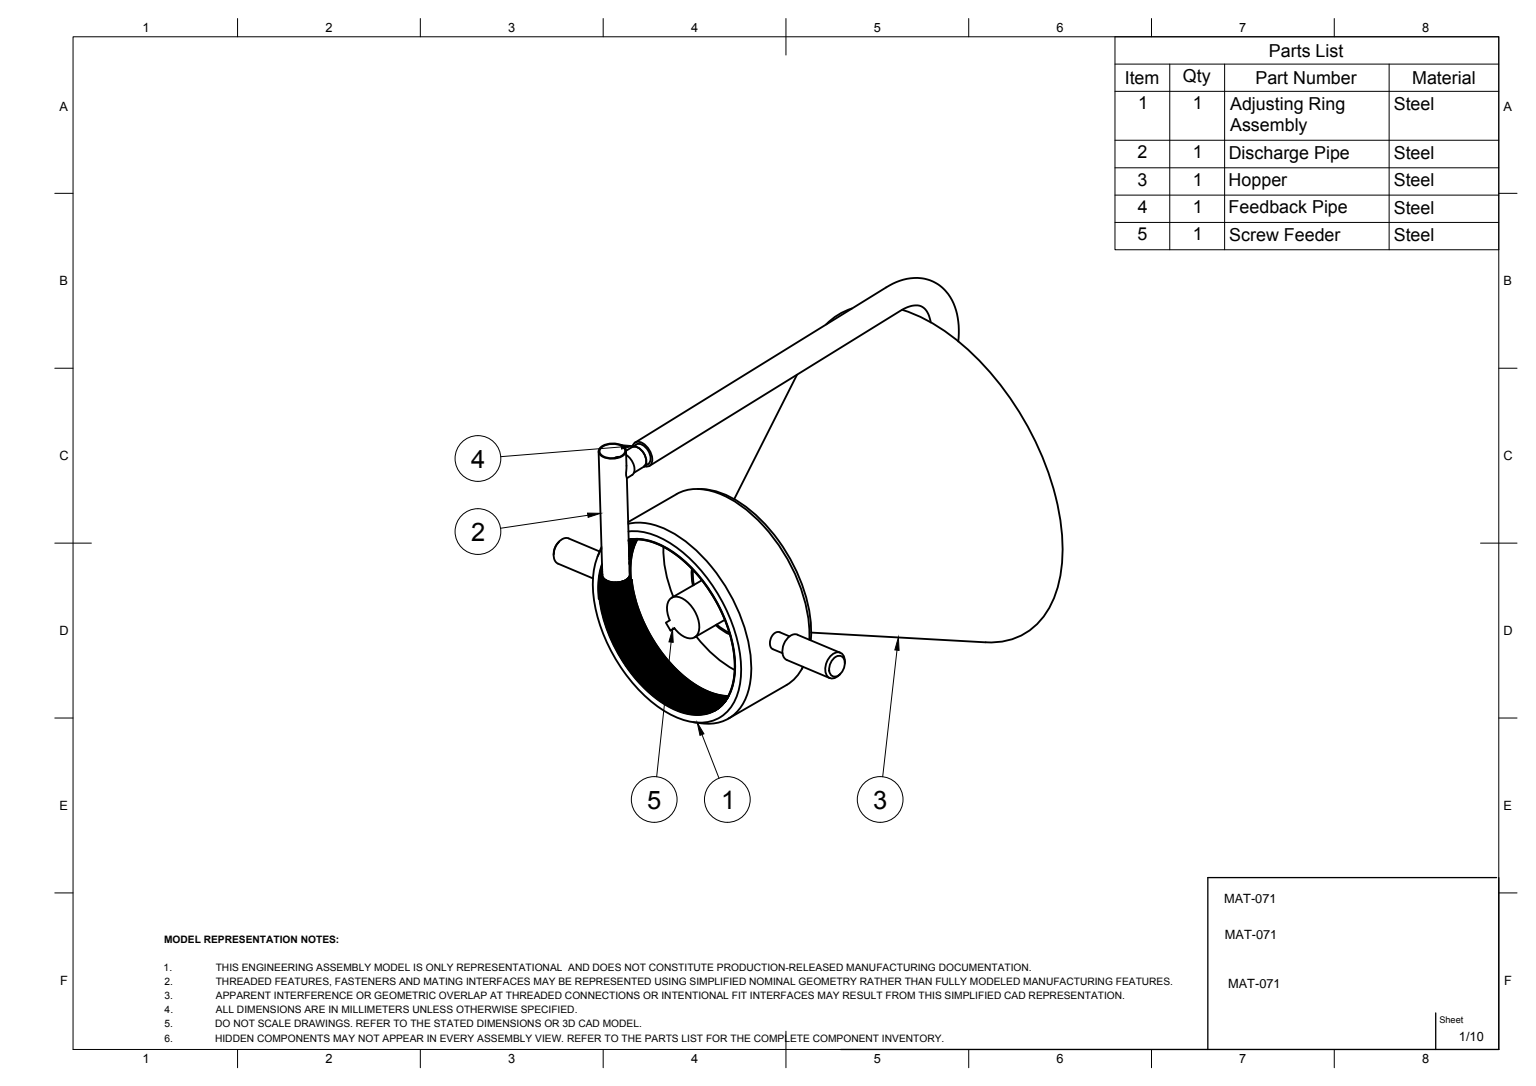
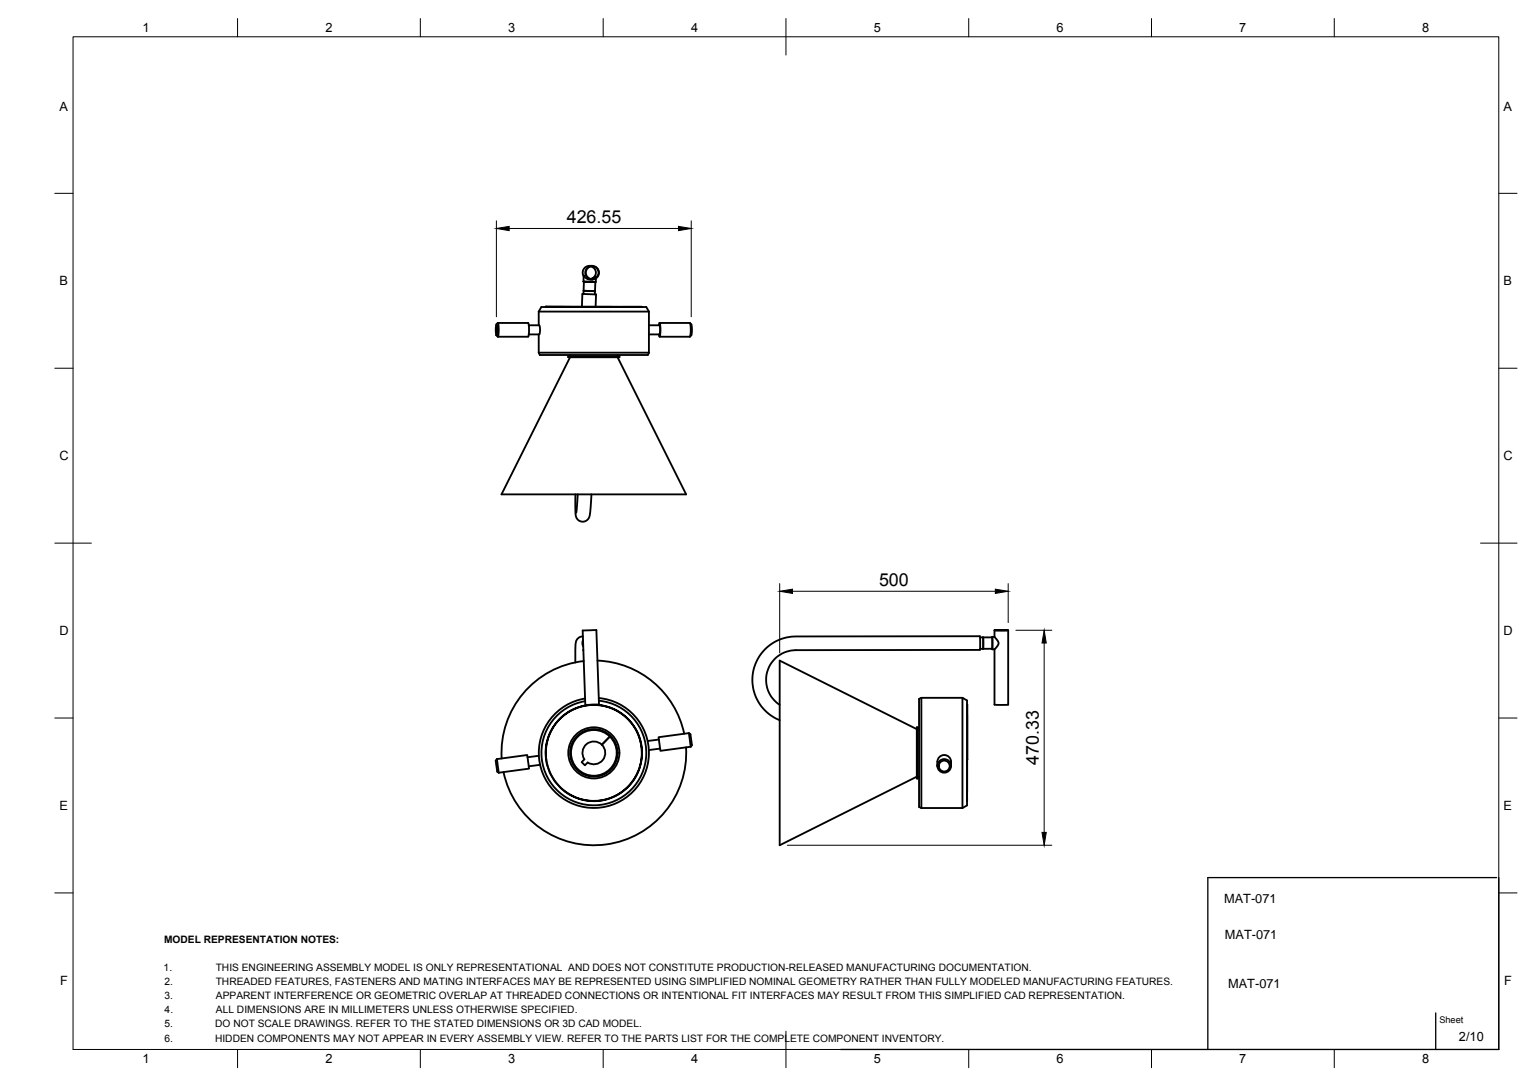
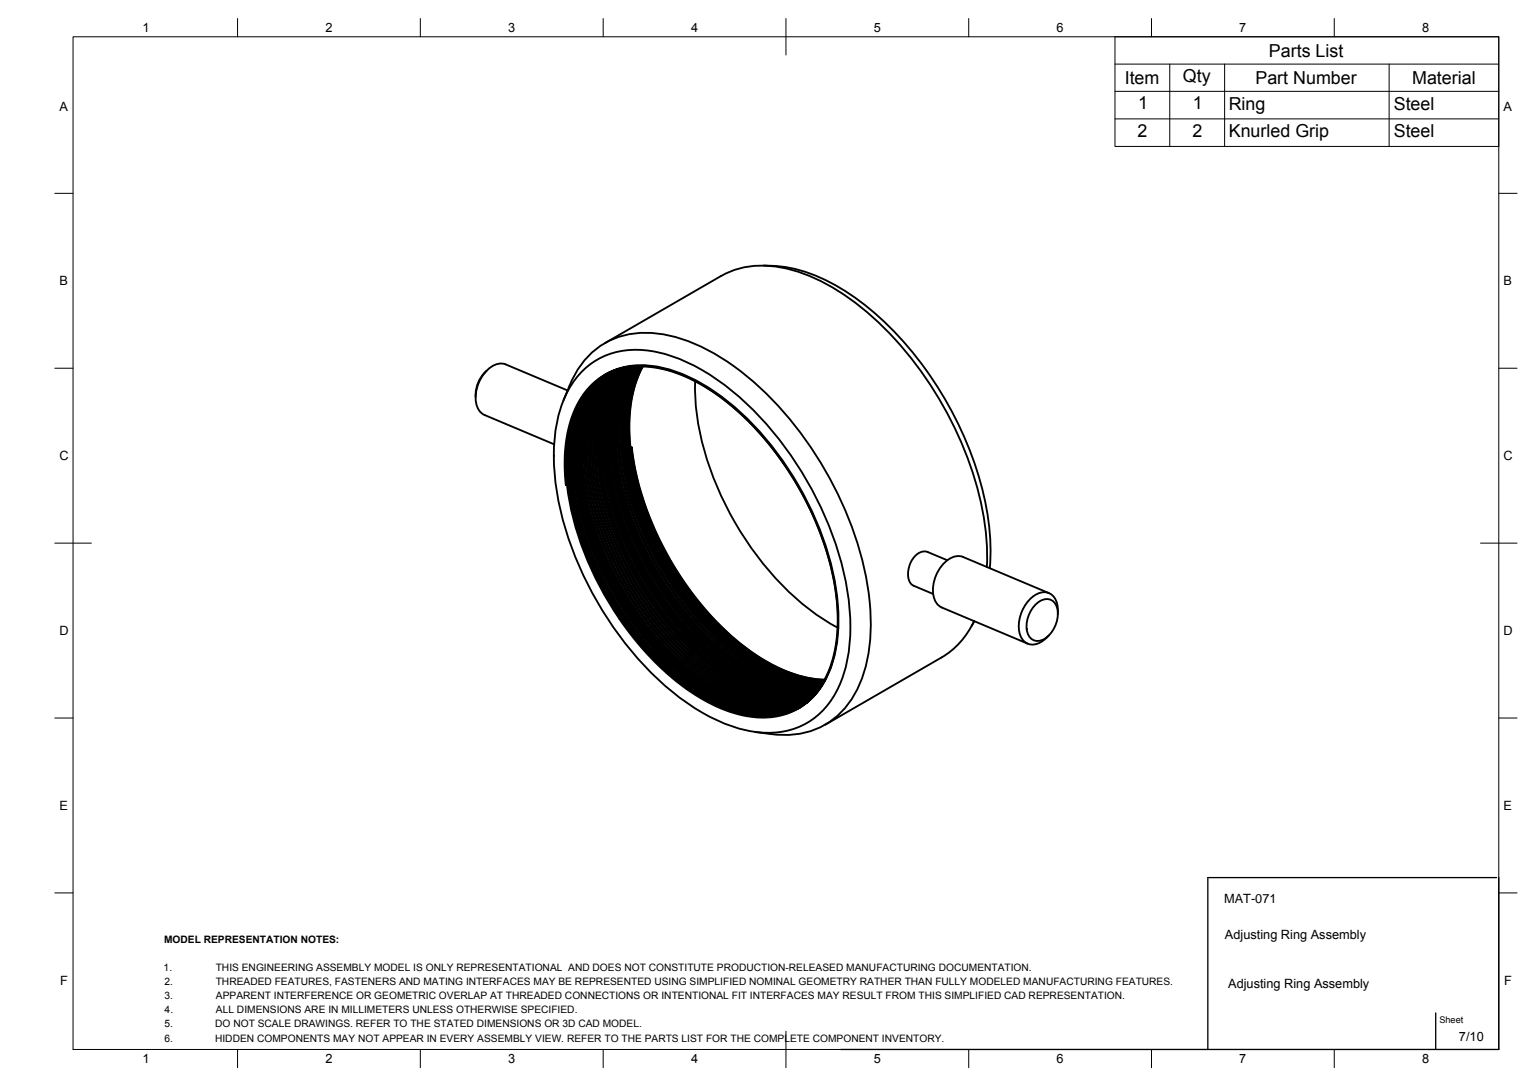
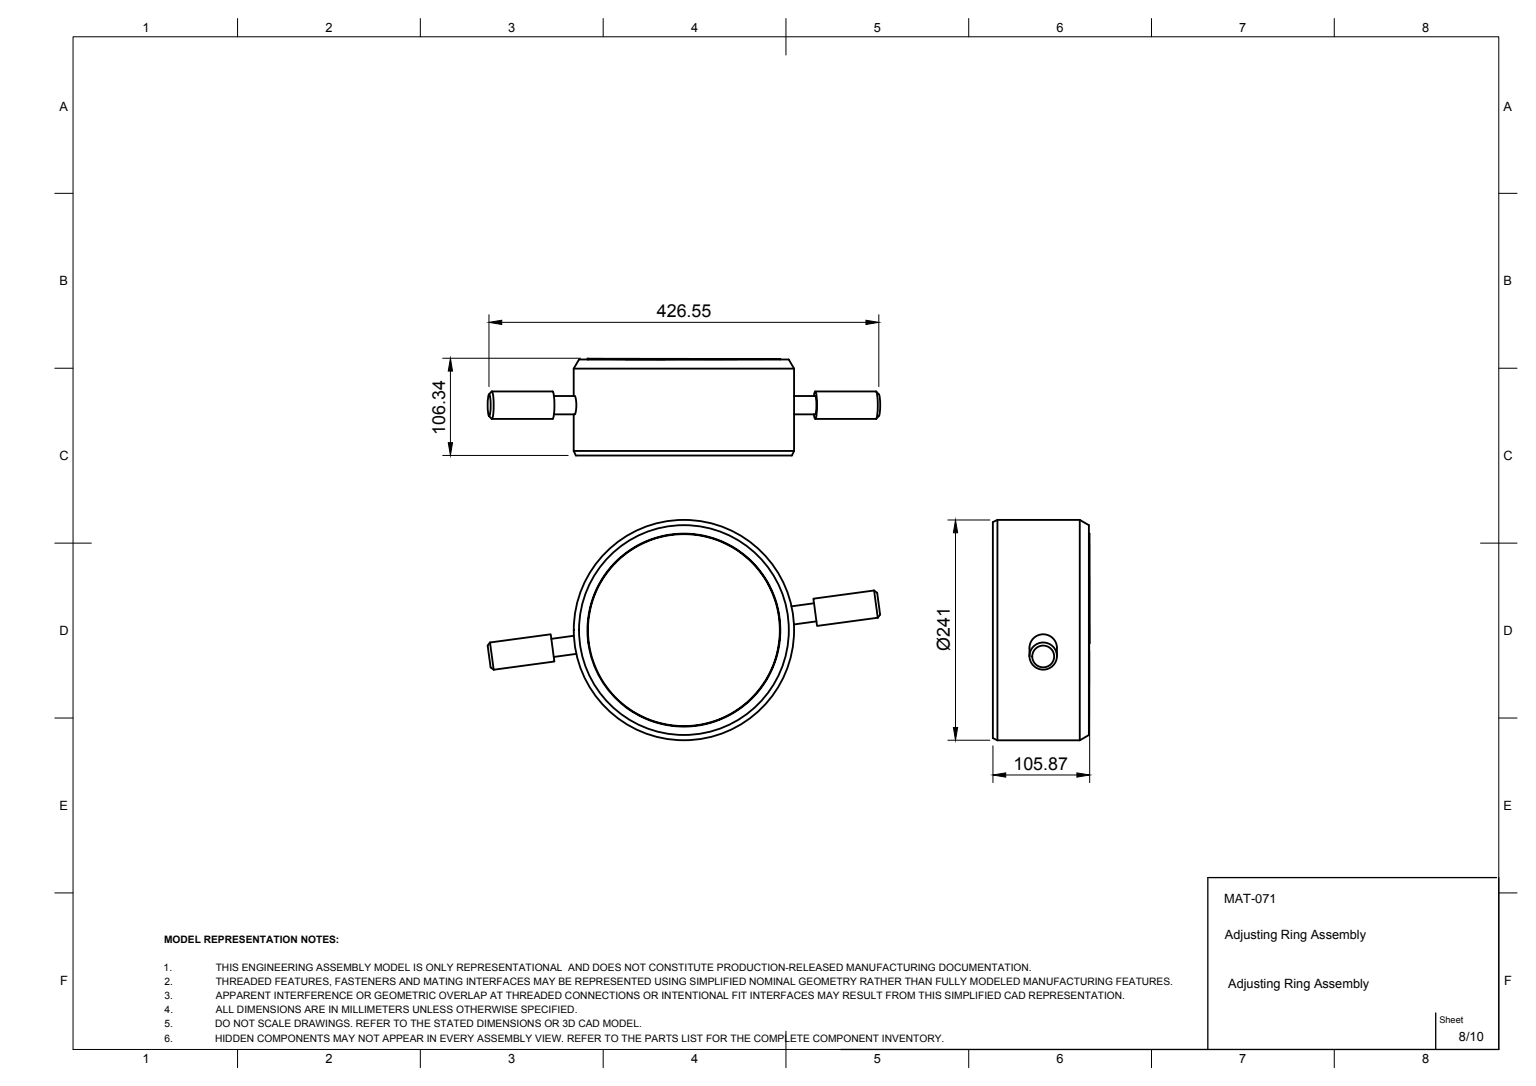
ISO-10303-21;
HEADER;
/* Generated by software containing ST-Developer
 * from STEP Tools, Inc. (www.steptools.com) 
 */

FILE_DESCRIPTION(
/* description */ (''),
/* implementation_level */ '2;1');

FILE_NAME(
/* name */ 'MAT-071',
/* time_stamp */ '2026-10-24T12:24:47-07:00',
/* author */ (''),
/* organization */ (''),
/* preprocessor_version */ 'ST-DEVELOPER v20.2',
/* originating_system */ 'Autodesk Translation Framework v15.15.0.0',
/* authorisation */ '');

FILE_SCHEMA (('AUTOMOTIVE_DESIGN { 1 0 10303 214 3 1 1 }'));
ENDSEC;

DATA;
#10=MECHANICAL_DESIGN_GEOMETRIC_PRESENTATION_REPRESENTATION('',(#57,#58,
#59,#60,#61,#62),#13594);
#11=TOROIDAL_SURFACE('',#3227,80.0000000000001,15.);
#12=TOROIDAL_SURFACE('',#3233,80.0000000000001,14.);
#13=ITEM_DEFINED_TRANSFORMATION($,$,#3039,#3179);
#14=ITEM_DEFINED_TRANSFORMATION($,$,#3167,#3180);
#15=ITEM_DEFINED_TRANSFORMATION($,$,#3167,#3181);
#16=ITEM_DEFINED_TRANSFORMATION($,$,#3038,#3271);
#17=ITEM_DEFINED_TRANSFORMATION($,$,#3182,#3272);
#18=ITEM_DEFINED_TRANSFORMATION($,$,#3204,#3273);
#19=ITEM_DEFINED_TRANSFORMATION($,$,#3223,#3274);
#20=ITEM_DEFINED_TRANSFORMATION($,$,#3252,#3275);
#21=(
REPRESENTATION_RELATIONSHIP($,$,#13625,#13624)
REPRESENTATION_RELATIONSHIP_WITH_TRANSFORMATION(#13)
SHAPE_REPRESENTATION_RELATIONSHIP()
);
#22=(
REPRESENTATION_RELATIONSHIP($,$,#13626,#13624)
REPRESENTATION_RELATIONSHIP_WITH_TRANSFORMATION(#14)
SHAPE_REPRESENTATION_RELATIONSHIP()
);
#23=(
REPRESENTATION_RELATIONSHIP($,$,#13626,#13624)
REPRESENTATION_RELATIONSHIP_WITH_TRANSFORMATION(#15)
SHAPE_REPRESENTATION_RELATIONSHIP()
);
#24=(
REPRESENTATION_RELATIONSHIP($,$,#13624,#13623)
REPRESENTATION_RELATIONSHIP_WITH_TRANSFORMATION(#16)
SHAPE_REPRESENTATION_RELATIONSHIP()
);
#25=(
REPRESENTATION_RELATIONSHIP($,$,#13627,#13623)
REPRESENTATION_RELATIONSHIP_WITH_TRANSFORMATION(#17)
SHAPE_REPRESENTATION_RELATIONSHIP()
);
#26=(
REPRESENTATION_RELATIONSHIP($,$,#13628,#13623)
REPRESENTATION_RELATIONSHIP_WITH_TRANSFORMATION(#18)
SHAPE_REPRESENTATION_RELATIONSHIP()
);
#27=(
REPRESENTATION_RELATIONSHIP($,$,#13629,#13623)
REPRESENTATION_RELATIONSHIP_WITH_TRANSFORMATION(#19)
SHAPE_REPRESENTATION_RELATIONSHIP()
);
#28=(
REPRESENTATION_RELATIONSHIP($,$,#13630,#13623)
REPRESENTATION_RELATIONSHIP_WITH_TRANSFORMATION(#20)
SHAPE_REPRESENTATION_RELATIONSHIP()
);
#29=CONTEXT_DEPENDENT_SHAPE_REPRESENTATION(#21,#13611);
#30=CONTEXT_DEPENDENT_SHAPE_REPRESENTATION(#22,#13612);
#31=CONTEXT_DEPENDENT_SHAPE_REPRESENTATION(#23,#13613);
#32=CONTEXT_DEPENDENT_SHAPE_REPRESENTATION(#24,#13618);
#33=CONTEXT_DEPENDENT_SHAPE_REPRESENTATION(#25,#13619);
#34=CONTEXT_DEPENDENT_SHAPE_REPRESENTATION(#26,#13620);
#35=CONTEXT_DEPENDENT_SHAPE_REPRESENTATION(#27,#13621);
#36=CONTEXT_DEPENDENT_SHAPE_REPRESENTATION(#28,#13622);
#37=NEXT_ASSEMBLY_USAGE_OCCURRENCE('Ring:1','Ring:1','Ring:1',#13633,#13634,
'Ring:1');
#38=NEXT_ASSEMBLY_USAGE_OCCURRENCE('Knurled Grip:1','Knurled Grip:1',
'Knurled Grip:1',#13633,#13635,'Knurled Grip:1');
#39=NEXT_ASSEMBLY_USAGE_OCCURRENCE('Knurled Grip:2','Knurled Grip:2',
'Knurled Grip:2',#13633,#13635,'Knurled Grip:2');
#40=NEXT_ASSEMBLY_USAGE_OCCURRENCE('Adjusting Ring Assembly:1',
'Adjusting Ring Assembly:1','Adjusting Ring Assembly:1',#13632,#13633,
'Adjusting Ring Assembly:1');
#41=NEXT_ASSEMBLY_USAGE_OCCURRENCE('Discharge Pipe:1',
'Discharge Pipe:1','Discharge Pipe:1',#13632,#13636,'Discharge Pipe:1');
#42=NEXT_ASSEMBLY_USAGE_OCCURRENCE('Hopper:1','Hopper:1','Hopper:1',#13632,
#13637,'Hopper:1');
#43=NEXT_ASSEMBLY_USAGE_OCCURRENCE('Feedback Pipe:1','Feedback Pipe:1',
'Feedback Pipe:1',#13632,#13638,'Feedback Pipe:1');
#44=NEXT_ASSEMBLY_USAGE_OCCURRENCE('Screw Feeder:1','Screw Feeder:1',
'Screw Feeder:1',#13632,#13639,'Screw Feeder:1');
#45=SHAPE_REPRESENTATION_RELATIONSHIP('SRR','None',#13625,#51);
#46=SHAPE_REPRESENTATION_RELATIONSHIP('SRR','None',#13626,#52);
#47=SHAPE_REPRESENTATION_RELATIONSHIP('SRR','None',#13627,#53);
#48=SHAPE_REPRESENTATION_RELATIONSHIP('SRR','None',#13628,#54);
#49=SHAPE_REPRESENTATION_RELATIONSHIP('SRR','None',#13629,#55);
#50=SHAPE_REPRESENTATION_RELATIONSHIP('SRR','None',#13630,#56);
#51=ADVANCED_BREP_SHAPE_REPRESENTATION('',(#63),#13588);
#52=ADVANCED_BREP_SHAPE_REPRESENTATION('',(#64),#13589);
#53=ADVANCED_BREP_SHAPE_REPRESENTATION('',(#65),#13590);
#54=ADVANCED_BREP_SHAPE_REPRESENTATION('',(#66),#13591);
#55=ADVANCED_BREP_SHAPE_REPRESENTATION('',(#67),#13592);
#56=ADVANCED_BREP_SHAPE_REPRESENTATION('',(#68),#13593);
#57=STYLED_ITEM('',(#13667),#63);
#58=STYLED_ITEM('',(#13667),#64);
#59=STYLED_ITEM('',(#13667),#65);
#60=STYLED_ITEM('',(#13667),#66);
#61=STYLED_ITEM('',(#13667),#67);
#62=STYLED_ITEM('',(#13667),#68);
#63=MANIFOLD_SOLID_BREP('Ring',#2964);
#64=MANIFOLD_SOLID_BREP('Knurled Grip',#2965);
#65=MANIFOLD_SOLID_BREP('Discharge Pipe 2',#2966);
#66=MANIFOLD_SOLID_BREP('Hopper',#2967);
#67=MANIFOLD_SOLID_BREP('Feedback Pipe',#2968);
#68=MANIFOLD_SOLID_BREP('Screw Feeder',#2969);
#69=(
BOUNDED_SURFACE()
B_SPLINE_SURFACE(1,2,((#7782,#7783,#7784,#7785,#7786,#7787,#7788,#7789,
#7790,#7791,#7792,#7793,#7794,#7795,#7796,#7797,#7798,#7799,#7800,#7801,
#7802,#7803,#7804,#7805,#7806,#7807,#7808,#7809,#7810,#7811,#7812,#7813,
#7814,#7815,#7816,#7817,#7818,#7819,#7820,#7821,#7822,#7823,#7824,#7825,
#7826,#7827,#7828,#7829,#7830,#7831,#7832,#7833,#7834,#7835,#7836,#7837,
#7838,#7839,#7840,#7841,#7842,#7843,#7844,#7845,#7846,#7847,#7848,#7849,
#7850,#7851,#7852,#7853,#7854,#7855,#7856,#7857,#7858,#7859,#7860,#7861,
#7862,#7863,#7864,#7865,#7866,#7867,#7868,#7869,#7870,#7871,#7872,#7873,
#7874,#7875,#7876,#7877,#7878,#7879,#7880,#7881,#7882,#7883,#7884,#7885,
#7886,#7887,#7888,#7889,#7890,#7891,#7892,#7893,#7894,#7895,#7896,#7897,
#7898,#7899,#7900,#7901,#7902,#7903,#7904,#7905,#7906,#7907,#7908,#7909,
#7910,#7911,#7912,#7913,#7914,#7915,#7916,#7917,#7918,#7919,#7920,#7921,
#7922,#7923,#7924,#7925,#7926,#7927,#7928,#7929,#7930,#7931,#7932,#7933,
#7934,#7935,#7936,#7937,#7938,#7939,#7940,#7941,#7942,#7943,#7944,#7945,
#7946,#7947,#7948,#7949,#7950,#7951,#7952,#7953,#7954,#7955,#7956,#7957,
#7958,#7959,#7960,#7961,#7962,#7963,#7964,#7965,#7966,#7967,#7968,#7969,
#7970,#7971,#7972,#7973,#7974,#7975,#7976,#7977,#7978,#7979,#7980,#7981,
#7982,#7983,#7984,#7985,#7986,#7987,#7988,#7989,#7990,#7991,#7992,#7993,
#7994,#7995,#7996,#7997,#7998,#7999,#8000,#8001,#8002,#8003,#8004,#8005,
#8006,#8007,#8008,#8009,#8010,#8011,#8012,#8013,#8014,#8015,#8016,#8017,
#8018,#8019,#8020,#8021,#8022,#8023,#8024,#8025,#8026,#8027,#8028,#8029,
#8030,#8031,#8032,#8033,#8034,#8035,#8036,#8037,#8038,#8039,#8040,#8041,
#8042,#8043,#8044,#8045,#8046,#8047,#8048,#8049,#8050,#8051,#8052,#8053,
#8054,#8055,#8056,#8057,#8058,#8059,#8060,#8061,#8062,#8063,#8064,#8065,
#8066,#8067,#8068,#8069,#8070,#8071,#8072,#8073,#8074,#8075,#8076,#8077,
#8078,#8079,#8080,#8081,#8082,#8083,#8084,#8085,#8086,#8087,#8088,#8089,
#8090,#8091,#8092,#8093,#8094,#8095,#8096,#8097,#8098,#8099,#8100,#8101,
#8102,#8103,#8104,#8105,#8106,#8107,#8108,#8109,#8110,#8111,#8112,#8113,
#8114,#8115,#8116,#8117,#8118,#8119,#8120,#8121,#8122,#8123,#8124,#8125,
#8126,#8127,#8128,#8129,#8130,#8131,#8132,#8133,#8134,#8135,#8136,#8137,
#8138,#8139,#8140,#8141,#8142,#8143,#8144,#8145,#8146,#8147,#8148,#8149,
#8150,#8151,#8152,#8153,#8154,#8155,#8156,#8157,#8158,#8159,#8160,#8161,
#8162,#8163,#8164,#8165,#8166,#8167,#8168,#8169,#8170,#8171,#8172,#8173,
#8174,#8175,#8176,#8177,#8178,#8179,#8180,#8181,#8182,#8183,#8184,#8185,
#8186,#8187,#8188,#8189,#8190,#8191,#8192,#8193,#8194,#8195,#8196,#8197,
#8198,#8199,#8200,#8201,#8202,#8203,#8204,#8205,#8206,#8207,#8208,#8209,
#8210,#8211,#8212,#8213,#8214,#8215,#8216,#8217,#8218,#8219,#8220,#8221,
#8222,#8223,#8224,#8225,#8226,#8227,#8228,#8229,#8230,#8231,#8232,#8233,
#8234,#8235,#8236,#8237,#8238,#8239,#8240,#8241,#8242,#8243,#8244,#8245,
#8246,#8247,#8248,#8249,#8250,#8251,#8252,#8253,#8254,#8255,#8256,#8257,
#8258,#8259,#8260,#8261,#8262,#8263,#8264,#8265,#8266,#8267,#8268,#8269,
#8270,#8271,#8272,#8273,#8274,#8275,#8276,#8277,#8278,#8279,#8280,#8281,
#8282,#8283,#8284,#8285,#8286,#8287,#8288,#8289,#8290,#8291,#8292,#8293,
#8294,#8295,#8296,#8297,#8298,#8299,#8300,#8301,#8302,#8303,#8304,#8305,
#8306,#8307,#8308,#8309,#8310,#8311,#8312,#8313,#8314,#8315,#8316,#8317,
#8318,#8319,#8320,#8321,#8322,#8323,#8324,#8325,#8326,#8327,#8328,#8329,
#8330,#8331,#8332,#8333,#8334,#8335,#8336,#8337,#8338,#8339,#8340,#8341,
#8342,#8343,#8344,#8345,#8346,#8347,#8348,#8349,#8350,#8351,#8352,#8353,
#8354,#8355,#8356,#8357,#8358,#8359,#8360,#8361,#8362,#8363,#8364,#8365,
#8366,#8367,#8368,#8369,#8370,#8371,#8372,#8373,#8374,#8375,#8376,#8377,
#8378,#8379,#8380,#8381,#8382,#8383,#8384,#8385,#8386,#8387,#8388,#8389,
#8390,#8391,#8392,#8393,#8394,#8395,#8396,#8397,#8398,#8399,#8400,#8401,
#8402,#8403,#8404,#8405,#8406,#8407,#8408,#8409,#8410,#8411,#8412,#8413,
#8414,#8415,#8416,#8417,#8418,#8419,#8420,#8421,#8422,#8423,#8424,#8425,
#8426,#8427,#8428,#8429,#8430,#8431,#8432,#8433,#8434,#8435,#8436,#8437,
#8438,#8439,#8440,#8441,#8442,#8443,#8444,#8445,#8446,#8447,#8448,#8449,
#8450,#8451,#8452,#8453,#8454,#8455,#8456,#8457,#8458,#8459,#8460,#8461,
#8462,#8463,#8464,#8465,#8466,#8467,#8468,#8469,#8470,#8471,#8472,#8473,
#8474,#8475,#8476,#8477,#8478,#8479,#8480,#8481,#8482,#8483,#8484,#8485,
#8486,#8487,#8488,#8489,#8490,#8491,#8492,#8493,#8494,#8495,#8496,#8497,
#8498,#8499,#8500,#8501,#8502,#8503,#8504,#8505,#8506,#8507,#8508,#8509,
#8510,#8511,#8512,#8513,#8514,#8515,#8516,#8517,#8518,#8519,#8520,#8521,
#8522,#8523,#8524,#8525,#8526,#8527,#8528,#8529,#8530,#8531,#8532,#8533,
#8534,#8535,#8536,#8537,#8538,#8539,#8540,#8541,#8542,#8543,#8544,#8545,
#8546,#8547,#8548,#8549,#8550,#8551,#8552,#8553,#8554,#8555,#8556,#8557,
#8558,#8559,#8560,#8561,#8562,#8563,#8564,#8565,#8566,#8567,#8568,#8569,
#8570,#8571,#8572,#8573,#8574,#8575,#8576,#8577,#8578,#8579,#8580,#8581,
#8582),(#8583,#8584,#8585,#8586,#8587,#8588,#8589,#8590,#8591,#8592,#8593,
#8594,#8595,#8596,#8597,#8598,#8599,#8600,#8601,#8602,#8603,#8604,#8605,
#8606,#8607,#8608,#8609,#8610,#8611,#8612,#8613,#8614,#8615,#8616,#8617,
#8618,#8619,#8620,#8621,#8622,#8623,#8624,#8625,#8626,#8627,#8628,#8629,
#8630,#8631,#8632,#8633,#8634,#8635,#8636,#8637,#8638,#8639,#8640,#8641,
#8642,#8643,#8644,#8645,#8646,#8647,#8648,#8649,#8650,#8651,#8652,#8653,
#8654,#8655,#8656,#8657,#8658,#8659,#8660,#8661,#8662,#8663,#8664,#8665,
#8666,#8667,#8668,#8669,#8670,#8671,#8672,#8673,#8674,#8675,#8676,#8677,
#8678,#8679,#8680,#8681,#8682,#8683,#8684,#8685,#8686,#8687,#8688,#8689,
#8690,#8691,#8692,#8693,#8694,#8695,#8696,#8697,#8698,#8699,#8700,#8701,
#8702,#8703,#8704,#8705,#8706,#8707,#8708,#8709,#8710,#8711,#8712,#8713,
#8714,#8715,#8716,#8717,#8718,#8719,#8720,#8721,#8722,#8723,#8724,#8725,
#8726,#8727,#8728,#8729,#8730,#8731,#8732,#8733,#8734,#8735,#8736,#8737,
#8738,#8739,#8740,#8741,#8742,#8743,#8744,#8745,#8746,#8747,#8748,#8749,
#8750,#8751,#8752,#8753,#8754,#8755,#8756,#8757,#8758,#8759,#8760,#8761,
#8762,#8763,#8764,#8765,#8766,#8767,#8768,#8769,#8770,#8771,#8772,#8773,
#8774,#8775,#8776,#8777,#8778,#8779,#8780,#8781,#8782,#8783,#8784,#8785,
#8786,#8787,#8788,#8789,#8790,#8791,#8792,#8793,#8794,#8795,#8796,#8797,
#8798,#8799,#8800,#8801,#8802,#8803,#8804,#8805,#8806,#8807,#8808,#8809,
#8810,#8811,#8812,#8813,#8814,#8815,#8816,#8817,#8818,#8819,#8820,#8821,
#8822,#8823,#8824,#8825,#8826,#8827,#8828,#8829,#8830,#8831,#8832,#8833,
#8834,#8835,#8836,#8837,#8838,#8839,#8840,#8841,#8842,#8843,#8844,#8845,
#8846,#8847,#8848,#8849,#8850,#8851,#8852,#8853,#8854,#8855,#8856,#8857,
#8858,#8859,#8860,#8861,#8862,#8863,#8864,#8865,#8866,#8867,#8868,#8869,
#8870,#8871,#8872,#8873,#8874,#8875,#8876,#8877,#8878,#8879,#8880,#8881,
#8882,#8883,#8884,#8885,#8886,#8887,#8888,#8889,#8890,#8891,#8892,#8893,
#8894,#8895,#8896,#8897,#8898,#8899,#8900,#8901,#8902,#8903,#8904,#8905,
#8906,#8907,#8908,#8909,#8910,#8911,#8912,#8913,#8914,#8915,#8916,#8917,
#8918,#8919,#8920,#8921,#8922,#8923,#8924,#8925,#8926,#8927,#8928,#8929,
#8930,#8931,#8932,#8933,#8934,#8935,#8936,#8937,#8938,#8939,#8940,#8941,
#8942,#8943,#8944,#8945,#8946,#8947,#8948,#8949,#8950,#8951,#8952,#8953,
#8954,#8955,#8956,#8957,#8958,#8959,#8960,#8961,#8962,#8963,#8964,#8965,
#8966,#8967,#8968,#8969,#8970,#8971,#8972,#8973,#8974,#8975,#8976,#8977,
#8978,#8979,#8980,#8981,#8982,#8983,#8984,#8985,#8986,#8987,#8988,#8989,
#8990,#8991,#8992,#8993,#8994,#8995,#8996,#8997,#8998,#8999,#9000,#9001,
#9002,#9003,#9004,#9005,#9006,#9007,#9008,#9009,#9010,#9011,#9012,#9013,
#9014,#9015,#9016,#9017,#9018,#9019,#9020,#9021,#9022,#9023,#9024,#9025,
#9026,#9027,#9028,#9029,#9030,#9031,#9032,#9033,#9034,#9035,#9036,#9037,
#9038,#9039,#9040,#9041,#9042,#9043,#9044,#9045,#9046,#9047,#9048,#9049,
#9050,#9051,#9052,#9053,#9054,#9055,#9056,#9057,#9058,#9059,#9060,#9061,
#9062,#9063,#9064,#9065,#9066,#9067,#9068,#9069,#9070,#9071,#9072,#9073,
#9074,#9075,#9076,#9077,#9078,#9079,#9080,#9081,#9082,#9083,#9084,#9085,
#9086,#9087,#9088,#9089,#9090,#9091,#9092,#9093,#9094,#9095,#9096,#9097,
#9098,#9099,#9100,#9101,#9102,#9103,#9104,#9105,#9106,#9107,#9108,#9109,
#9110,#9111,#9112,#9113,#9114,#9115,#9116,#9117,#9118,#9119,#9120,#9121,
#9122,#9123,#9124,#9125,#9126,#9127,#9128,#9129,#9130,#9131,#9132,#9133,
#9134,#9135,#9136,#9137,#9138,#9139,#9140,#9141,#9142,#9143,#9144,#9145,
#9146,#9147,#9148,#9149,#9150,#9151,#9152,#9153,#9154,#9155,#9156,#9157,
#9158,#9159,#9160,#9161,#9162,#9163,#9164,#9165,#9166,#9167,#9168,#9169,
#9170,#9171,#9172,#9173,#9174,#9175,#9176,#9177,#9178,#9179,#9180,#9181,
#9182,#9183,#9184,#9185,#9186,#9187,#9188,#9189,#9190,#9191,#9192,#9193,
#9194,#9195,#9196,#9197,#9198,#9199,#9200,#9201,#9202,#9203,#9204,#9205,
#9206,#9207,#9208,#9209,#9210,#9211,#9212,#9213,#9214,#9215,#9216,#9217,
#9218,#9219,#9220,#9221,#9222,#9223,#9224,#9225,#9226,#9227,#9228,#9229,
#9230,#9231,#9232,#9233,#9234,#9235,#9236,#9237,#9238,#9239,#9240,#9241,
#9242,#9243,#9244,#9245,#9246,#9247,#9248,#9249,#9250,#9251,#9252,#9253,
#9254,#9255,#9256,#9257,#9258,#9259,#9260,#9261,#9262,#9263,#9264,#9265,
#9266,#9267,#9268,#9269,#9270,#9271,#9272,#9273,#9274,#9275,#9276,#9277,
#9278,#9279,#9280,#9281,#9282,#9283,#9284,#9285,#9286,#9287,#9288,#9289,
#9290,#9291,#9292,#9293,#9294,#9295,#9296,#9297,#9298,#9299,#9300,#9301,
#9302,#9303,#9304,#9305,#9306,#9307,#9308,#9309,#9310,#9311,#9312,#9313,
#9314,#9315,#9316,#9317,#9318,#9319,#9320,#9321,#9322,#9323,#9324,#9325,
#9326,#9327,#9328,#9329,#9330,#9331,#9332,#9333,#9334,#9335,#9336,#9337,
#9338,#9339,#9340,#9341,#9342,#9343,#9344,#9345,#9346,#9347,#9348,#9349,
#9350,#9351,#9352,#9353,#9354,#9355,#9356,#9357,#9358,#9359,#9360,#9361,
#9362,#9363,#9364,#9365,#9366,#9367,#9368,#9369,#9370,#9371,#9372,#9373,
#9374,#9375,#9376,#9377,#9378,#9379,#9380,#9381,#9382,#9383)),
 .UNSPECIFIED.,.F.,.F.,.F.)
B_SPLINE_SURFACE_WITH_KNOTS((2,2),(3,2,2,2,2,2,2,2,2,2,2,2,2,2,2,2,2,2,
2,2,2,2,2,2,2,2,2,2,2,2,2,2,2,2,2,2,2,2,2,2,2,2,2,2,2,2,2,2,2,2,2,2,2,2,
2,2,2,2,2,2,2,2,2,2,2,2,2,2,2,2,2,2,2,2,2,2,2,2,2,2,2,2,2,2,2,2,2,2,2,2,
2,2,2,2,2,2,2,2,2,2,2,2,2,2,2,2,2,2,2,2,2,2,2,2,2,2,2,2,2,2,2,2,2,2,2,2,
2,2,2,2,2,2,2,2,2,2,2,2,2,2,2,2,2,2,2,2,2,2,2,2,2,2,2,2,2,2,2,2,2,2,2,2,
2,2,2,2,2,2,2,2,2,2,2,2,2,2,2,2,2,2,2,2,2,2,2,2,2,2,2,2,2,2,2,2,2,2,2,2,
2,2,2,2,2,2,2,2,2,2,2,2,2,2,2,2,2,2,2,2,2,2,2,2,2,2,2,2,2,2,2,2,2,2,2,2,
2,2,2,2,2,2,2,2,2,2,2,2,2,2,2,2,2,2,2,2,2,2,2,2,2,2,2,2,2,2,2,2,2,2,2,2,
2,2,2,2,2,2,2,2,2,2,2,2,2,2,2,2,2,2,2,2,2,2,2,2,2,2,2,2,2,2,2,2,2,2,2,2,
2,2,2,2,2,2,2,2,2,2,2,2,2,2,2,2,2,2,2,2,2,2,2,2,2,2,2,2,2,2,2,2,2,2,2,2,
2,2,2,2,2,2,2,2,2,2,2,2,2,2,2,2,2,2,2,2,2,2,2,2,2,2,2,2,2,2,2,2,2,2,2,2,
2,2,2,2,2,2,2,2,2,2,2,2,2,2,2,2,2,2,2,2,2,2,3),(0.,1.),(0.,0.0025,0.005,
0.0075,0.01,0.0125,0.015,0.0175,0.02,0.0225,0.025,0.0275,0.03,0.0325,0.035,
0.0375,0.04,0.0425,0.045,0.0475,0.05,0.0525,0.055,0.0575,0.06,0.0625,0.065,
0.0675,0.07,0.0725,0.075,0.0775,0.08,0.0825,0.085,0.0875,0.09,0.0925,0.095,
0.0975,0.1,0.1025,0.105,0.1075,0.11,0.1125,0.115,0.1175,0.12,0.1225,0.125,
0.1275,0.13,0.1325,0.135,0.1375,0.14,0.1425,0.145,0.1475,0.15,0.1525,0.155,
0.1575,0.16,0.1625,0.165,0.1675,0.17,0.1725,0.175,0.1775,0.18,0.1825,0.185,
0.1875,0.19,0.1925,0.195,0.1975,0.2,0.2025,0.205,0.2075,0.21,0.2125,0.215,
0.2175,0.22,0.2225,0.225,0.2275,0.23,0.2325,0.235,0.2375,0.24,0.2425,0.245,
0.2475,0.25,0.2525,0.255,0.2575,0.26,0.2625,0.265,0.2675,0.27,0.2725,0.275,
0.2775,0.28,0.2825,0.285,0.2875,0.29,0.2925,0.295,0.2975,0.3,0.3025,0.305,
0.3075,0.31,0.3125,0.315,0.3175,0.32,0.3225,0.325,0.3275,0.33,0.3325,0.335,
0.3375,0.34,0.3425,0.345,0.3475,0.35,0.3525,0.355,0.3575,0.36,0.3625,0.365,
0.3675,0.37,0.3725,0.375,0.3775,0.38,0.3825,0.385,0.3875,0.39,0.3925,0.395,
0.3975,0.4,0.4025,0.405,0.4075,0.41,0.4125,0.415,0.4175,0.42,0.4225,0.425,
0.4275,0.43,0.4325,0.435,0.4375,0.44,0.4425,0.445,0.4475,0.45,0.4525,0.455,
0.4575,0.46,0.4625,0.465,0.4675,0.47,0.4725,0.475,0.4775,0.48,0.4825,0.485,
0.4875,0.49,0.4925,0.495,0.4975,0.5,0.5025,0.505,0.5075,0.51,0.5125,0.515,
0.5175,0.52,0.5225,0.525,0.5275,0.53,0.5325,0.535,0.5375,0.54,0.5425,0.545,
0.5475,0.55,0.5525,0.555,0.5575,0.56,0.5625,0.565,0.5675,0.57,0.5725,0.575,
0.5775,0.58,0.5825,0.585,0.5875,0.59,0.5925,0.595,0.5975,0.6,0.6025,0.605,
0.6075,0.61,0.6125,0.615,0.6175,0.62,0.6225,0.625,0.6275,0.63,0.6325,0.635,
0.6375,0.64,0.6425,0.645,0.6475,0.65,0.6525,0.655,0.6575,0.66,0.6625,0.665,
0.6675,0.67,0.6725,0.675,0.6775,0.68,0.6825,0.685,0.6875,0.69,0.6925,0.695,
0.6975,0.7,0.7025,0.705,0.7075,0.71,0.7125,0.715,0.7175,0.72,0.7225,0.725,
0.7275,0.73,0.7325,0.735,0.7375,0.74,0.7425,0.745,0.7475,0.75,0.7525,0.755,
0.7575,0.76,0.7625,0.765,0.7675,0.77,0.7725,0.775,0.7775,0.78,0.7825,0.785,
0.7875,0.79,0.7925,0.795,0.7975,0.8,0.8025,0.805,0.8075,0.81,0.8125,0.815,
0.8175,0.82,0.8225,0.825,0.8275,0.83,0.8325,0.835,0.8375,0.84,0.8425,0.845,
0.8475,0.85,0.8525,0.855,0.8575,0.86,0.8625,0.865,0.8675,0.87,0.8725,0.875,
0.8775,0.88,0.8825,0.885,0.8875,0.89,0.8925,0.895,0.8975,0.9,0.9025,0.905,
0.9075,0.91,0.9125,0.915,0.9175,0.92,0.9225,0.925,0.9275,0.93,0.9325,0.935,
0.9375,0.94,0.9425,0.945,0.9475,0.95,0.9525,0.955,0.9575,0.96,0.9625,0.965,
0.9675,0.97,0.9725,0.975,0.9775,0.98,0.9825,0.985,0.9875,0.99,0.9925,0.995,
0.9975,1.),.UNSPECIFIED.)
GEOMETRIC_REPRESENTATION_ITEM()
RATIONAL_B_SPLINE_SURFACE(((1.,0.923879532511287,1.,0.923879532511287,1.,
0.923879532511287,1.,0.923879532511287,1.,0.923879532511287,1.,0.923879532511287,
1.,0.923879532511287,1.,0.923879532511287,1.,0.923879532511287,1.,0.923879532511287,
1.,0.923879532511287,1.,0.923879532511287,1.,0.923879532511287,1.,0.923879532511287,
1.,0.923879532511287,1.,0.923879532511287,1.,0.923879532511287,1.,0.923879532511287,
1.,0.923879532511287,1.,0.923879532511287,1.,0.923879532511287,1.,0.923879532511287,
1.,0.923879532511287,1.,0.923879532511287,1.,0.923879532511287,1.,0.923879532511287,
1.,0.923879532511287,1.,0.923879532511287,1.,0.923879532511287,1.,0.923879532511287,
1.,0.923879532511287,1.,0.923879532511287,1.,0.923879532511287,1.,0.923879532511287,
1.,0.923879532511287,1.,0.923879532511287,1.,0.923879532511287,1.,0.923879532511287,
1.,0.923879532511287,1.,0.923879532511287,1.,0.923879532511287,1.,0.923879532511287,
1.,0.923879532511287,1.,0.923879532511287,1.,0.923879532511287,1.,0.923879532511287,
1.,0.923879532511287,1.,0.923879532511287,1.,0.923879532511287,1.,0.923879532511287,
1.,0.923879532511287,1.,0.923879532511287,1.,0.923879532511287,1.,0.923879532511287,
1.,0.923879532511287,1.,0.923879532511287,1.,0.923879532511287,1.,0.923879532511287,
1.,0.923879532511287,1.,0.923879532511287,1.,0.923879532511287,1.,0.923879532511287,
1.,0.923879532511287,1.,0.923879532511287,1.,0.923879532511287,1.,0.923879532511287,
1.,0.923879532511287,1.,0.923879532511287,1.,0.923879532511287,1.,0.923879532511287,
1.,0.923879532511287,1.,0.923879532511287,1.,0.923879532511287,1.,0.923879532511287,
1.,0.923879532511287,1.,0.923879532511287,1.,0.923879532511287,1.,0.923879532511287,
1.,0.923879532511287,1.,0.923879532511287,1.,0.923879532511287,1.,0.923879532511287,
1.,0.923879532511287,1.,0.923879532511287,1.,0.923879532511287,1.,0.923879532511287,
1.,0.923879532511287,1.,0.923879532511287,1.,0.923879532511287,1.,0.923879532511287,
1.,0.923879532511287,1.,0.923879532511287,1.,0.923879532511287,1.,0.923879532511287,
1.,0.923879532511287,1.,0.923879532511287,1.,0.923879532511287,1.,0.923879532511287,
1.,0.923879532511287,1.,0.923879532511287,1.,0.923879532511287,1.,0.923879532511287,
1.,0.923879532511287,1.,0.923879532511287,1.,0.923879532511287,1.,0.923879532511287,
1.,0.923879532511287,1.,0.923879532511287,1.,0.923879532511287,1.,0.923879532511287,
1.,0.923879532511287,1.,0.923879532511287,1.,0.923879532511287,1.,0.923879532511287,
1.,0.923879532511287,1.,0.923879532511287,1.,0.923879532511287,1.,0.923879532511287,
1.,0.923879532511287,1.,0.923879532511287,1.,0.923879532511287,1.,0.923879532511287,
1.,0.923879532511287,1.,0.923879532511287,1.,0.923879532511287,1.,0.923879532511287,
1.,0.923879532511287,1.,0.923879532511287,1.,0.923879532511287,1.,0.923879532511287,
1.,0.923879532511287,1.,0.923879532511287,1.,0.923879532511287,1.,0.923879532511287,
1.,0.923879532511287,1.,0.923879532511287,1.,0.923879532511287,1.,0.923879532511287,
1.,0.923879532511287,1.,0.923879532511287,1.,0.923879532511287,1.,0.923879532511287,
1.,0.923879532511287,1.,0.923879532511287,1.,0.923879532511287,1.,0.923879532511287,
1.,0.923879532511287,1.,0.923879532511287,1.,0.923879532511287,1.,0.923879532511287,
1.,0.923879532511287,1.,0.923879532511287,1.,0.923879532511287,1.,0.923879532511287,
1.,0.923879532511287,1.,0.923879532511287,1.,0.923879532511287,1.,0.923879532511287,
1.,0.923879532511287,1.,0.923879532511287,1.,0.923879532511287,1.,0.923879532511287,
1.,0.923879532511287,1.,0.923879532511287,1.,0.923879532511287,1.,0.923879532511287,
1.,0.923879532511287,1.,0.923879532511287,1.,0.923879532511287,1.,0.923879532511287,
1.,0.923879532511287,1.,0.923879532511287,1.,0.923879532511287,1.,0.923879532511287,
1.,0.923879532511287,1.,0.923879532511287,1.,0.923879532511287,1.,0.923879532511287,
1.,0.923879532511287,1.,0.923879532511287,1.,0.923879532511287,1.,0.923879532511287,
1.,0.923879532511287,1.,0.923879532511287,1.,0.923879532511287,1.,0.923879532511287,
1.,0.923879532511287,1.,0.923879532511287,1.,0.923879532511287,1.,0.923879532511287,
1.,0.923879532511287,1.,0.923879532511287,1.,0.923879532511287,1.,0.923879532511287,
1.,0.923879532511287,1.,0.923879532511287,1.,0.923879532511287,1.,0.923879532511287,
1.,0.923879532511287,1.,0.923879532511287,1.,0.923879532511287,1.,0.923879532511287,
1.,0.923879532511287,1.,0.923879532511287,1.,0.923879532511287,1.,0.923879532511287,
1.,0.923879532511287,1.,0.923879532511287,1.,0.923879532511287,1.,0.923879532511287,
1.,0.923879532511287,1.,0.923879532511287,1.,0.923879532511287,1.,0.923879532511287,
1.,0.923879532511287,1.,0.923879532511287,1.,0.923879532511287,1.,0.923879532511287,
1.,0.923879532511287,1.,0.923879532511287,1.,0.923879532511287,1.,0.923879532511287,
1.,0.923879532511287,1.,0.923879532511287,1.,0.923879532511287,1.,0.923879532511287,
1.,0.923879532511287,1.,0.923879532511287,1.,0.923879532511287,1.,0.923879532511287,
1.,0.923879532511287,1.,0.923879532511287,1.,0.923879532511287,1.,0.923879532511287,
1.,0.923879532511287,1.,0.923879532511287,1.,0.923879532511287,1.,0.923879532511287,
1.,0.923879532511287,1.,0.923879532511287,1.,0.923879532511287,1.,0.923879532511287,
1.,0.923879532511287,1.,0.923879532511287,1.,0.923879532511287,1.,0.923879532511287,
1.,0.923879532511287,1.,0.923879532511287,1.,0.923879532511287,1.,0.923879532511287,
1.,0.923879532511287,1.,0.923879532511287,1.,0.923879532511287,1.,0.923879532511287,
1.,0.923879532511287,1.,0.923879532511287,1.,0.923879532511287,1.,0.923879532511287,
1.,0.923879532511287,1.,0.923879532511287,1.,0.923879532511287,1.,0.923879532511287,
1.,0.923879532511287,1.,0.923879532511287,1.,0.923879532511287,1.,0.923879532511287,
1.,0.923879532511287,1.,0.923879532511287,1.,0.923879532511287,1.,0.923879532511287,
1.,0.923879532511287,1.,0.923879532511287,1.,0.923879532511287,1.,0.923879532511287,
1.,0.923879532511287,1.,0.923879532511287,1.,0.923879532511287,1.,0.923879532511287,
1.,0.923879532511287,1.,0.923879532511287,1.,0.923879532511287,1.,0.923879532511287,
1.,0.923879532511287,1.,0.923879532511287,1.,0.923879532511287,1.,0.923879532511287,
1.,0.923879532511287,1.,0.923879532511287,1.,0.923879532511287,1.,0.923879532511287,
1.,0.923879532511287,1.,0.923879532511287,1.,0.923879532511287,1.,0.923879532511287,
1.,0.923879532511287,1.,0.923879532511287,1.,0.923879532511287,1.,0.923879532511287,
1.,0.923879532511287,1.,0.923879532511287,1.,0.923879532511287,1.,0.923879532511287,
1.,0.923879532511287,1.,0.923879532511287,1.,0.923879532511287,1.,0.923879532511287,
1.,0.923879532511287,1.,0.923879532511287,1.,0.923879532511287,1.,0.923879532511287,
1.,0.923879532511287,1.,0.923879532511287,1.,0.923879532511287,1.,0.923879532511287,
1.,0.923879532511287,1.,0.923879532511287,1.,0.923879532511287,1.,0.923879532511287,
1.,0.923879532511287,1.,0.923879532511287,1.,0.923879532511287,1.,0.923879532511287,
1.,0.923879532511287,1.,0.923879532511287,1.,0.923879532511287,1.,0.923879532511287,
1.,0.923879532511287,1.,0.923879532511287,1.,0.923879532511287,1.,0.923879532511287,
1.,0.923879532511287,1.,0.923879532511287,1.,0.923879532511287,1.,0.923879532511287,
1.,0.923879532511287,1.,0.923879532511287,1.,0.923879532511287,1.,0.923879532511287,
1.,0.923879532511287,1.,0.923879532511287,1.,0.923879532511287,1.,0.923879532511287,
1.,0.923879532511287,1.,0.923879532511287,1.,0.923879532511287,1.,0.923879532511287,
1.,0.923879532511287,1.,0.923879532511287,1.,0.923879532511287,1.,0.923879532511287,
1.,0.923879532511287,1.,0.923879532511287,1.,0.923879532511287,1.,0.923879532511287,
1.,0.923879532511287,1.,0.923879532511287,1.,0.923879532511287,1.,0.923879532511287,
1.,0.923879532511287,1.,0.923879532511287,1.,0.923879532511287,1.,0.923879532511287,
1.,0.923879532511287,1.,0.923879532511287,1.,0.923879532511287,1.,0.923879532511287,
1.,0.923879532511287,1.,0.923879532511287,1.,0.923879532511287,1.,0.923879532511287,
1.,0.923879532511287,1.,0.923879532511287,1.,0.923879532511287,1.,0.923879532511287,
1.,0.923879532511287,1.,0.923879532511287,1.,0.923879532511287,1.,0.923879532511287,
1.,0.923879532511287,1.,0.923879532511287,1.,0.923879532511287,1.,0.923879532511287,
1.,0.923879532511287,1.,0.923879532511287,1.,0.923879532511287,1.,0.923879532511287,
1.,0.923879532511287,1.,0.923879532511287,1.,0.923879532511287,1.,0.923879532511287,
1.,0.923879532511287,1.,0.923879532511287,1.,0.923879532511287,1.,0.923879532511287,
1.,0.923879532511287,1.,0.923879532511287,1.,0.923879532511287,1.,0.923879532511287,
1.,0.923879532511287,1.,0.923879532511287,1.),(1.,0.923879532511287,1.,
0.923879532511287,1.,0.923879532511287,1.,0.923879532511287,1.,0.923879532511287,
1.,0.923879532511287,1.,0.923879532511287,1.,0.923879532511287,1.,0.923879532511287,
1.,0.923879532511287,1.,0.923879532511287,1.,0.923879532511287,1.,0.923879532511287,
1.,0.923879532511287,1.,0.923879532511287,1.,0.923879532511287,1.,0.923879532511287,
1.,0.923879532511287,1.,0.923879532511287,1.,0.923879532511287,1.,0.923879532511287,
1.,0.923879532511287,1.,0.923879532511287,1.,0.923879532511287,1.,0.923879532511287,
1.,0.923879532511287,1.,0.923879532511287,1.,0.923879532511287,1.,0.923879532511287,
1.,0.923879532511287,1.,0.923879532511287,1.,0.923879532511287,1.,0.923879532511287,
1.,0.923879532511287,1.,0.923879532511287,1.,0.923879532511287,1.,0.923879532511287,
1.,0.923879532511287,1.,0.923879532511287,1.,0.923879532511287,1.,0.923879532511287,
1.,0.923879532511287,1.,0.923879532511287,1.,0.923879532511287,1.,0.923879532511287,
1.,0.923879532511287,1.,0.923879532511287,1.,0.923879532511287,1.,0.923879532511287,
1.,0.923879532511287,1.,0.923879532511287,1.,0.923879532511287,1.,0.923879532511287,
1.,0.923879532511287,1.,0.923879532511287,1.,0.923879532511287,1.,0.923879532511287,
1.,0.923879532511287,1.,0.923879532511287,1.,0.923879532511287,1.,0.923879532511287,
1.,0.923879532511287,1.,0.923879532511287,1.,0.923879532511287,1.,0.923879532511287,
1.,0.923879532511287,1.,0.923879532511287,1.,0.923879532511287,1.,0.923879532511287,
1.,0.923879532511287,1.,0.923879532511287,1.,0.923879532511287,1.,0.923879532511287,
1.,0.923879532511287,1.,0.923879532511287,1.,0.923879532511287,1.,0.923879532511287,
1.,0.923879532511287,1.,0.923879532511287,1.,0.923879532511287,1.,0.923879532511287,
1.,0.923879532511287,1.,0.923879532511287,1.,0.923879532511287,1.,0.923879532511287,
1.,0.923879532511287,1.,0.923879532511287,1.,0.923879532511287,1.,0.923879532511287,
1.,0.923879532511287,1.,0.923879532511287,1.,0.923879532511287,1.,0.923879532511287,
1.,0.923879532511287,1.,0.923879532511287,1.,0.923879532511287,1.,0.923879532511287,
1.,0.923879532511287,1.,0.923879532511287,1.,0.923879532511287,1.,0.923879532511287,
1.,0.923879532511287,1.,0.923879532511287,1.,0.923879532511287,1.,0.923879532511287,
1.,0.923879532511287,1.,0.923879532511287,1.,0.923879532511287,1.,0.923879532511287,
1.,0.923879532511287,1.,0.923879532511287,1.,0.923879532511287,1.,0.923879532511287,
1.,0.923879532511287,1.,0.923879532511287,1.,0.923879532511287,1.,0.923879532511287,
1.,0.923879532511287,1.,0.923879532511287,1.,0.923879532511287,1.,0.923879532511287,
1.,0.923879532511287,1.,0.923879532511287,1.,0.923879532511287,1.,0.923879532511287,
1.,0.923879532511287,1.,0.923879532511287,1.,0.923879532511287,1.,0.923879532511287,
1.,0.923879532511287,1.,0.923879532511287,1.,0.923879532511287,1.,0.923879532511287,
1.,0.923879532511287,1.,0.923879532511287,1.,0.923879532511287,1.,0.923879532511287,
1.,0.923879532511287,1.,0.923879532511287,1.,0.923879532511287,1.,0.923879532511287,
1.,0.923879532511287,1.,0.923879532511287,1.,0.923879532511287,1.,0.923879532511287,
1.,0.923879532511287,1.,0.923879532511287,1.,0.923879532511287,1.,0.923879532511287,
1.,0.923879532511287,1.,0.923879532511287,1.,0.923879532511287,1.,0.923879532511287,
1.,0.923879532511287,1.,0.923879532511287,1.,0.923879532511287,1.,0.923879532511287,
1.,0.923879532511287,1.,0.923879532511287,1.,0.923879532511287,1.,0.923879532511287,
1.,0.923879532511287,1.,0.923879532511287,1.,0.923879532511287,1.,0.923879532511287,
1.,0.923879532511287,1.,0.923879532511287,1.,0.923879532511287,1.,0.923879532511287,
1.,0.923879532511287,1.,0.923879532511287,1.,0.923879532511287,1.,0.923879532511287,
1.,0.923879532511287,1.,0.923879532511287,1.,0.923879532511287,1.,0.923879532511287,
1.,0.923879532511287,1.,0.923879532511287,1.,0.923879532511287,1.,0.923879532511287,
1.,0.923879532511287,1.,0.923879532511287,1.,0.923879532511287,1.,0.923879532511287,
1.,0.923879532511287,1.,0.923879532511287,1.,0.923879532511287,1.,0.923879532511287,
1.,0.923879532511287,1.,0.923879532511287,1.,0.923879532511287,1.,0.923879532511287,
1.,0.923879532511287,1.,0.923879532511287,1.,0.923879532511287,1.,0.923879532511287,
1.,0.923879532511287,1.,0.923879532511287,1.,0.923879532511287,1.,0.923879532511287,
1.,0.923879532511287,1.,0.923879532511287,1.,0.923879532511287,1.,0.923879532511287,
1.,0.923879532511287,1.,0.923879532511287,1.,0.923879532511287,1.,0.923879532511287,
1.,0.923879532511287,1.,0.923879532511287,1.,0.923879532511287,1.,0.923879532511287,
1.,0.923879532511287,1.,0.923879532511287,1.,0.923879532511287,1.,0.923879532511287,
1.,0.923879532511287,1.,0.923879532511287,1.,0.923879532511287,1.,0.923879532511287,
1.,0.923879532511287,1.,0.923879532511287,1.,0.923879532511287,1.,0.923879532511287,
1.,0.923879532511287,1.,0.923879532511287,1.,0.923879532511287,1.,0.923879532511287,
1.,0.923879532511287,1.,0.923879532511287,1.,0.923879532511287,1.,0.923879532511287,
1.,0.923879532511287,1.,0.923879532511287,1.,0.923879532511287,1.,0.923879532511287,
1.,0.923879532511287,1.,0.923879532511287,1.,0.923879532511287,1.,0.923879532511287,
1.,0.923879532511287,1.,0.923879532511287,1.,0.923879532511287,1.,0.923879532511287,
1.,0.923879532511287,1.,0.923879532511287,1.,0.923879532511287,1.,0.923879532511287,
1.,0.923879532511287,1.,0.923879532511287,1.,0.923879532511287,1.,0.923879532511287,
1.,0.923879532511287,1.,0.923879532511287,1.,0.923879532511287,1.,0.923879532511287,
1.,0.923879532511287,1.,0.923879532511287,1.,0.923879532511287,1.,0.923879532511287,
1.,0.923879532511287,1.,0.923879532511287,1.,0.923879532511287,1.,0.923879532511287,
1.,0.923879532511287,1.,0.923879532511287,1.,0.923879532511287,1.,0.923879532511287,
1.,0.923879532511287,1.,0.923879532511287,1.,0.923879532511287,1.,0.923879532511287,
1.,0.923879532511287,1.,0.923879532511287,1.,0.923879532511287,1.,0.923879532511287,
1.,0.923879532511287,1.,0.923879532511287,1.,0.923879532511287,1.,0.923879532511287,
1.,0.923879532511287,1.,0.923879532511287,1.,0.923879532511287,1.,0.923879532511287,
1.,0.923879532511287,1.,0.923879532511287,1.,0.923879532511287,1.,0.923879532511287,
1.,0.923879532511287,1.,0.923879532511287,1.,0.923879532511287,1.,0.923879532511287,
1.,0.923879532511287,1.,0.923879532511287,1.,0.923879532511287,1.,0.923879532511287,
1.,0.923879532511287,1.,0.923879532511287,1.,0.923879532511287,1.,0.923879532511287,
1.,0.923879532511287,1.,0.923879532511287,1.,0.923879532511287,1.,0.923879532511287,
1.,0.923879532511287,1.,0.923879532511287,1.,0.923879532511287,1.,0.923879532511287,
1.,0.923879532511287,1.,0.923879532511287,1.,0.923879532511287,1.,0.923879532511287,
1.,0.923879532511287,1.,0.923879532511287,1.,0.923879532511287,1.,0.923879532511287,
1.,0.923879532511287,1.,0.923879532511287,1.,0.923879532511287,1.,0.923879532511287,
1.,0.923879532511287,1.,0.923879532511287,1.,0.923879532511287,1.,0.923879532511287,
1.,0.923879532511287,1.,0.923879532511287,1.,0.923879532511287,1.,0.923879532511287,
1.,0.923879532511287,1.,0.923879532511287,1.,0.923879532511287,1.,0.923879532511287,
1.,0.923879532511287,1.,0.923879532511287,1.,0.923879532511287,1.,0.923879532511287,
1.,0.923879532511287,1.,0.923879532511287,1.,0.923879532511287,1.,0.923879532511287,
1.,0.923879532511287,1.,0.923879532511287,1.,0.923879532511287,1.,0.923879532511287,
1.,0.923879532511287,1.,0.923879532511287,1.,0.923879532511287,1.,0.923879532511287,
1.,0.923879532511287,1.,0.923879532511287,1.,0.923879532511287,1.,0.923879532511287,
1.,0.923879532511287,1.,0.923879532511287,1.,0.923879532511287,1.,0.923879532511287,
1.,0.923879532511287,1.,0.923879532511287,1.,0.923879532511287,1.,0.923879532511287,
1.,0.923879532511287,1.,0.923879532511287,1.,0.923879532511287,1.,0.923879532511287,
1.,0.923879532511287,1.,0.923879532511287,1.,0.923879532511287,1.,0.923879532511287,
1.,0.923879532511287,1.,0.923879532511287,1.,0.923879532511287,1.,0.923879532511287,
1.,0.923879532511287,1.,0.923879532511287,1.,0.923879532511287,1.,0.923879532511287,
1.,0.923879532511287,1.,0.923879532511287,1.,0.923879532511287,1.,0.923879532511287,
1.,0.923879532511287,1.,0.923879532511287,1.,0.923879532511287,1.,0.923879532511287,
1.,0.923879532511287,1.,0.923879532511287,1.,0.923879532511287,1.,0.923879532511287,
1.,0.923879532511287,1.,0.923879532511287,1.,0.923879532511287,1.,0.923879532511287,
1.,0.923879532511287,1.,0.923879532511287,1.,0.923879532511287,1.,0.923879532511287,
1.,0.923879532511287,1.,0.923879532511287,1.,0.923879532511287,1.)))
REPRESENTATION_ITEM('')
SURFACE()
);
#70=(
BOUNDED_SURFACE()
B_SPLINE_SURFACE(1,2,((#9419,#9420,#9421,#9422,#9423,#9424,#9425,#9426,
#9427,#9428,#9429,#9430,#9431,#9432,#9433,#9434,#9435,#9436,#9437,#9438,
#9439,#9440,#9441,#9442,#9443,#9444,#9445,#9446,#9447,#9448,#9449,#9450,
#9451,#9452,#9453,#9454,#9455,#9456,#9457,#9458,#9459,#9460,#9461,#9462,
#9463,#9464,#9465,#9466,#9467,#9468,#9469,#9470,#9471,#9472,#9473,#9474,
#9475,#9476,#9477,#9478,#9479,#9480,#9481,#9482,#9483,#9484,#9485,#9486,
#9487,#9488,#9489,#9490,#9491,#9492,#9493,#9494,#9495,#9496,#9497,#9498,
#9499,#9500,#9501,#9502,#9503,#9504,#9505,#9506,#9507,#9508,#9509,#9510,
#9511,#9512,#9513,#9514,#9515,#9516,#9517,#9518,#9519,#9520,#9521,#9522,
#9523,#9524,#9525,#9526,#9527,#9528,#9529,#9530,#9531,#9532,#9533,#9534,
#9535,#9536,#9537,#9538,#9539,#9540,#9541,#9542,#9543,#9544,#9545,#9546,
#9547,#9548,#9549,#9550,#9551,#9552,#9553,#9554,#9555,#9556,#9557,#9558,
#9559,#9560,#9561,#9562,#9563,#9564,#9565,#9566,#9567,#9568,#9569,#9570,
#9571,#9572,#9573,#9574,#9575,#9576,#9577,#9578,#9579,#9580,#9581,#9582,
#9583,#9584,#9585,#9586,#9587,#9588,#9589,#9590,#9591,#9592,#9593,#9594,
#9595,#9596,#9597,#9598,#9599,#9600,#9601,#9602,#9603,#9604,#9605,#9606,
#9607,#9608,#9609,#9610,#9611,#9612,#9613,#9614,#9615,#9616,#9617,#9618,
#9619,#9620,#9621,#9622,#9623,#9624,#9625,#9626,#9627,#9628,#9629,#9630,
#9631,#9632,#9633,#9634,#9635,#9636,#9637,#9638,#9639,#9640,#9641,#9642,
#9643,#9644,#9645,#9646,#9647,#9648,#9649,#9650,#9651,#9652,#9653,#9654,
#9655,#9656,#9657,#9658,#9659,#9660,#9661,#9662,#9663,#9664,#9665,#9666,
#9667,#9668,#9669,#9670,#9671,#9672,#9673,#9674,#9675,#9676,#9677,#9678,
#9679,#9680,#9681,#9682,#9683,#9684,#9685,#9686,#9687,#9688,#9689,#9690,
#9691,#9692,#9693,#9694,#9695,#9696,#9697,#9698,#9699,#9700,#9701,#9702,
#9703,#9704,#9705,#9706,#9707,#9708,#9709,#9710,#9711,#9712,#9713,#9714,
#9715,#9716,#9717,#9718,#9719,#9720,#9721,#9722,#9723,#9724,#9725,#9726,
#9727,#9728,#9729,#9730,#9731,#9732,#9733,#9734,#9735,#9736,#9737,#9738,
#9739,#9740,#9741,#9742,#9743,#9744,#9745,#9746,#9747,#9748,#9749,#9750,
#9751,#9752,#9753,#9754,#9755,#9756,#9757,#9758,#9759,#9760,#9761,#9762,
#9763,#9764,#9765,#9766,#9767,#9768,#9769,#9770,#9771,#9772,#9773,#9774,
#9775,#9776,#9777,#9778,#9779,#9780,#9781,#9782,#9783,#9784,#9785,#9786,
#9787,#9788,#9789,#9790,#9791,#9792,#9793,#9794,#9795,#9796,#9797,#9798,
#9799,#9800,#9801,#9802,#9803,#9804,#9805,#9806,#9807,#9808,#9809,#9810,
#9811,#9812,#9813,#9814,#9815,#9816,#9817,#9818,#9819,#9820,#9821,#9822,
#9823,#9824,#9825,#9826,#9827,#9828,#9829,#9830,#9831,#9832,#9833,#9834,
#9835,#9836,#9837,#9838,#9839,#9840,#9841,#9842,#9843,#9844,#9845,#9846,
#9847,#9848,#9849,#9850,#9851,#9852,#9853,#9854,#9855,#9856,#9857,#9858,
#9859,#9860,#9861,#9862,#9863,#9864,#9865,#9866,#9867,#9868,#9869,#9870,
#9871,#9872,#9873,#9874,#9875,#9876,#9877,#9878,#9879,#9880,#9881,#9882,
#9883,#9884,#9885,#9886,#9887,#9888,#9889,#9890,#9891,#9892,#9893,#9894,
#9895,#9896,#9897,#9898,#9899,#9900,#9901,#9902,#9903,#9904,#9905,#9906,
#9907,#9908,#9909,#9910,#9911,#9912,#9913,#9914,#9915,#9916,#9917,#9918,
#9919,#9920,#9921,#9922,#9923,#9924,#9925,#9926,#9927,#9928,#9929,#9930,
#9931,#9932,#9933,#9934,#9935,#9936,#9937,#9938,#9939,#9940,#9941,#9942,
#9943,#9944,#9945,#9946,#9947,#9948,#9949,#9950,#9951,#9952,#9953,#9954,
#9955,#9956,#9957,#9958,#9959,#9960,#9961,#9962,#9963,#9964,#9965,#9966,
#9967,#9968,#9969,#9970,#9971,#9972,#9973,#9974,#9975,#9976,#9977,#9978,
#9979,#9980,#9981,#9982,#9983,#9984,#9985,#9986,#9987,#9988,#9989,#9990,
#9991,#9992,#9993,#9994,#9995,#9996,#9997,#9998,#9999,#10000,#10001,#10002,
#10003,#10004,#10005,#10006,#10007,#10008,#10009,#10010,#10011,#10012,#10013,
#10014,#10015,#10016,#10017,#10018,#10019,#10020,#10021,#10022,#10023,#10024,
#10025,#10026,#10027,#10028,#10029,#10030,#10031,#10032,#10033,#10034,#10035,
#10036,#10037,#10038,#10039,#10040,#10041,#10042,#10043,#10044,#10045,#10046,
#10047,#10048,#10049,#10050,#10051,#10052,#10053,#10054,#10055,#10056,#10057,
#10058,#10059,#10060,#10061,#10062,#10063,#10064,#10065,#10066,#10067,#10068,
#10069,#10070,#10071,#10072,#10073,#10074,#10075,#10076,#10077,#10078,#10079,
#10080,#10081,#10082,#10083,#10084,#10085,#10086,#10087,#10088,#10089,#10090,
#10091,#10092,#10093,#10094,#10095,#10096,#10097,#10098,#10099,#10100,#10101,
#10102,#10103,#10104,#10105,#10106,#10107,#10108,#10109,#10110,#10111,#10112,
#10113,#10114,#10115,#10116,#10117,#10118,#10119,#10120,#10121,#10122,#10123,
#10124,#10125,#10126,#10127,#10128,#10129,#10130,#10131,#10132,#10133,#10134,
#10135,#10136,#10137,#10138,#10139,#10140,#10141,#10142,#10143,#10144,#10145,
#10146,#10147,#10148,#10149,#10150,#10151,#10152,#10153,#10154,#10155,#10156,
#10157,#10158,#10159,#10160,#10161,#10162,#10163,#10164,#10165,#10166,#10167,
#10168,#10169,#10170,#10171,#10172,#10173,#10174,#10175,#10176,#10177,#10178,
#10179,#10180,#10181,#10182,#10183,#10184,#10185,#10186,#10187,#10188,#10189,
#10190,#10191,#10192,#10193,#10194,#10195,#10196,#10197,#10198,#10199,#10200,
#10201,#10202,#10203,#10204,#10205,#10206,#10207,#10208,#10209,#10210,#10211,
#10212,#10213,#10214,#10215,#10216,#10217,#10218,#10219),(#10220,#10221,
#10222,#10223,#10224,#10225,#10226,#10227,#10228,#10229,#10230,#10231,#10232,
#10233,#10234,#10235,#10236,#10237,#10238,#10239,#10240,#10241,#10242,#10243,
#10244,#10245,#10246,#10247,#10248,#10249,#10250,#10251,#10252,#10253,#10254,
#10255,#10256,#10257,#10258,#10259,#10260,#10261,#10262,#10263,#10264,#10265,
#10266,#10267,#10268,#10269,#10270,#10271,#10272,#10273,#10274,#10275,#10276,
#10277,#10278,#10279,#10280,#10281,#10282,#10283,#10284,#10285,#10286,#10287,
#10288,#10289,#10290,#10291,#10292,#10293,#10294,#10295,#10296,#10297,#10298,
#10299,#10300,#10301,#10302,#10303,#10304,#10305,#10306,#10307,#10308,#10309,
#10310,#10311,#10312,#10313,#10314,#10315,#10316,#10317,#10318,#10319,#10320,
#10321,#10322,#10323,#10324,#10325,#10326,#10327,#10328,#10329,#10330,#10331,
#10332,#10333,#10334,#10335,#10336,#10337,#10338,#10339,#10340,#10341,#10342,
#10343,#10344,#10345,#10346,#10347,#10348,#10349,#10350,#10351,#10352,#10353,
#10354,#10355,#10356,#10357,#10358,#10359,#10360,#10361,#10362,#10363,#10364,
#10365,#10366,#10367,#10368,#10369,#10370,#10371,#10372,#10373,#10374,#10375,
#10376,#10377,#10378,#10379,#10380,#10381,#10382,#10383,#10384,#10385,#10386,
#10387,#10388,#10389,#10390,#10391,#10392,#10393,#10394,#10395,#10396,#10397,
#10398,#10399,#10400,#10401,#10402,#10403,#10404,#10405,#10406,#10407,#10408,
#10409,#10410,#10411,#10412,#10413,#10414,#10415,#10416,#10417,#10418,#10419,
#10420,#10421,#10422,#10423,#10424,#10425,#10426,#10427,#10428,#10429,#10430,
#10431,#10432,#10433,#10434,#10435,#10436,#10437,#10438,#10439,#10440,#10441,
#10442,#10443,#10444,#10445,#10446,#10447,#10448,#10449,#10450,#10451,#10452,
#10453,#10454,#10455,#10456,#10457,#10458,#10459,#10460,#10461,#10462,#10463,
#10464,#10465,#10466,#10467,#10468,#10469,#10470,#10471,#10472,#10473,#10474,
#10475,#10476,#10477,#10478,#10479,#10480,#10481,#10482,#10483,#10484,#10485,
#10486,#10487,#10488,#10489,#10490,#10491,#10492,#10493,#10494,#10495,#10496,
#10497,#10498,#10499,#10500,#10501,#10502,#10503,#10504,#10505,#10506,#10507,
#10508,#10509,#10510,#10511,#10512,#10513,#10514,#10515,#10516,#10517,#10518,
#10519,#10520,#10521,#10522,#10523,#10524,#10525,#10526,#10527,#10528,#10529,
#10530,#10531,#10532,#10533,#10534,#10535,#10536,#10537,#10538,#10539,#10540,
#10541,#10542,#10543,#10544,#10545,#10546,#10547,#10548,#10549,#10550,#10551,
#10552,#10553,#10554,#10555,#10556,#10557,#10558,#10559,#10560,#10561,#10562,
#10563,#10564,#10565,#10566,#10567,#10568,#10569,#10570,#10571,#10572,#10573,
#10574,#10575,#10576,#10577,#10578,#10579,#10580,#10581,#10582,#10583,#10584,
#10585,#10586,#10587,#10588,#10589,#10590,#10591,#10592,#10593,#10594,#10595,
#10596,#10597,#10598,#10599,#10600,#10601,#10602,#10603,#10604,#10605,#10606,
#10607,#10608,#10609,#10610,#10611,#10612,#10613,#10614,#10615,#10616,#10617,
#10618,#10619,#10620,#10621,#10622,#10623,#10624,#10625,#10626,#10627,#10628,
#10629,#10630,#10631,#10632,#10633,#10634,#10635,#10636,#10637,#10638,#10639,
#10640,#10641,#10642,#10643,#10644,#10645,#10646,#10647,#10648,#10649,#10650,
#10651,#10652,#10653,#10654,#10655,#10656,#10657,#10658,#10659,#10660,#10661,
#10662,#10663,#10664,#10665,#10666,#10667,#10668,#10669,#10670,#10671,#10672,
#10673,#10674,#10675,#10676,#10677,#10678,#10679,#10680,#10681,#10682,#10683,
#10684,#10685,#10686,#10687,#10688,#10689,#10690,#10691,#10692,#10693,#10694,
#10695,#10696,#10697,#10698,#10699,#10700,#10701,#10702,#10703,#10704,#10705,
#10706,#10707,#10708,#10709,#10710,#10711,#10712,#10713,#10714,#10715,#10716,
#10717,#10718,#10719,#10720,#10721,#10722,#10723,#10724,#10725,#10726,#10727,
#10728,#10729,#10730,#10731,#10732,#10733,#10734,#10735,#10736,#10737,#10738,
#10739,#10740,#10741,#10742,#10743,#10744,#10745,#10746,#10747,#10748,#10749,
#10750,#10751,#10752,#10753,#10754,#10755,#10756,#10757,#10758,#10759,#10760,
#10761,#10762,#10763,#10764,#10765,#10766,#10767,#10768,#10769,#10770,#10771,
#10772,#10773,#10774,#10775,#10776,#10777,#10778,#10779,#10780,#10781,#10782,
#10783,#10784,#10785,#10786,#10787,#10788,#10789,#10790,#10791,#10792,#10793,
#10794,#10795,#10796,#10797,#10798,#10799,#10800,#10801,#10802,#10803,#10804,
#10805,#10806,#10807,#10808,#10809,#10810,#10811,#10812,#10813,#10814,#10815,
#10816,#10817,#10818,#10819,#10820,#10821,#10822,#10823,#10824,#10825,#10826,
#10827,#10828,#10829,#10830,#10831,#10832,#10833,#10834,#10835,#10836,#10837,
#10838,#10839,#10840,#10841,#10842,#10843,#10844,#10845,#10846,#10847,#10848,
#10849,#10850,#10851,#10852,#10853,#10854,#10855,#10856,#10857,#10858,#10859,
#10860,#10861,#10862,#10863,#10864,#10865,#10866,#10867,#10868,#10869,#10870,
#10871,#10872,#10873,#10874,#10875,#10876,#10877,#10878,#10879,#10880,#10881,
#10882,#10883,#10884,#10885,#10886,#10887,#10888,#10889,#10890,#10891,#10892,
#10893,#10894,#10895,#10896,#10897,#10898,#10899,#10900,#10901,#10902,#10903,
#10904,#10905,#10906,#10907,#10908,#10909,#10910,#10911,#10912,#10913,#10914,
#10915,#10916,#10917,#10918,#10919,#10920,#10921,#10922,#10923,#10924,#10925,
#10926,#10927,#10928,#10929,#10930,#10931,#10932,#10933,#10934,#10935,#10936,
#10937,#10938,#10939,#10940,#10941,#10942,#10943,#10944,#10945,#10946,#10947,
#10948,#10949,#10950,#10951,#10952,#10953,#10954,#10955,#10956,#10957,#10958,
#10959,#10960,#10961,#10962,#10963,#10964,#10965,#10966,#10967,#10968,#10969,
#10970,#10971,#10972,#10973,#10974,#10975,#10976,#10977,#10978,#10979,#10980,
#10981,#10982,#10983,#10984,#10985,#10986,#10987,#10988,#10989,#10990,#10991,
#10992,#10993,#10994,#10995,#10996,#10997,#10998,#10999,#11000,#11001,#11002,
#11003,#11004,#11005,#11006,#11007,#11008,#11009,#11010,#11011,#11012,#11013,
#11014,#11015,#11016,#11017,#11018,#11019,#11020)),.UNSPECIFIED.,.F.,.F.,
 .F.)
B_SPLINE_SURFACE_WITH_KNOTS((2,2),(3,2,2,2,2,2,2,2,2,2,2,2,2,2,2,2,2,2,
2,2,2,2,2,2,2,2,2,2,2,2,2,2,2,2,2,2,2,2,2,2,2,2,2,2,2,2,2,2,2,2,2,2,2,2,
2,2,2,2,2,2,2,2,2,2,2,2,2,2,2,2,2,2,2,2,2,2,2,2,2,2,2,2,2,2,2,2,2,2,2,2,
2,2,2,2,2,2,2,2,2,2,2,2,2,2,2,2,2,2,2,2,2,2,2,2,2,2,2,2,2,2,2,2,2,2,2,2,
2,2,2,2,2,2,2,2,2,2,2,2,2,2,2,2,2,2,2,2,2,2,2,2,2,2,2,2,2,2,2,2,2,2,2,2,
2,2,2,2,2,2,2,2,2,2,2,2,2,2,2,2,2,2,2,2,2,2,2,2,2,2,2,2,2,2,2,2,2,2,2,2,
2,2,2,2,2,2,2,2,2,2,2,2,2,2,2,2,2,2,2,2,2,2,2,2,2,2,2,2,2,2,2,2,2,2,2,2,
2,2,2,2,2,2,2,2,2,2,2,2,2,2,2,2,2,2,2,2,2,2,2,2,2,2,2,2,2,2,2,2,2,2,2,2,
2,2,2,2,2,2,2,2,2,2,2,2,2,2,2,2,2,2,2,2,2,2,2,2,2,2,2,2,2,2,2,2,2,2,2,2,
2,2,2,2,2,2,2,2,2,2,2,2,2,2,2,2,2,2,2,2,2,2,2,2,2,2,2,2,2,2,2,2,2,2,2,2,
2,2,2,2,2,2,2,2,2,2,2,2,2,2,2,2,2,2,2,2,2,2,2,2,2,2,2,2,2,2,2,2,2,2,2,2,
2,2,2,2,2,2,2,2,2,2,2,2,2,2,2,2,2,2,2,2,2,2,3),(0.,1.),(0.,0.0025,0.005,
0.0075,0.01,0.0125,0.015,0.0175,0.02,0.0225,0.025,0.0275,0.03,0.0325,0.035,
0.0375,0.04,0.0425,0.045,0.0475,0.05,0.0525,0.055,0.0575,0.06,0.0625,0.065,
0.0675,0.07,0.0725,0.075,0.0775,0.08,0.0825,0.085,0.0875,0.09,0.0925,0.095,
0.0975,0.1,0.1025,0.105,0.1075,0.11,0.1125,0.115,0.1175,0.12,0.1225,0.125,
0.1275,0.13,0.1325,0.135,0.1375,0.14,0.1425,0.145,0.1475,0.15,0.1525,0.155,
0.1575,0.16,0.1625,0.165,0.1675,0.17,0.1725,0.175,0.1775,0.18,0.1825,0.185,
0.1875,0.19,0.1925,0.195,0.1975,0.2,0.2025,0.205,0.2075,0.21,0.2125,0.215,
0.2175,0.22,0.2225,0.225,0.2275,0.23,0.2325,0.235,0.2375,0.24,0.2425,0.245,
0.2475,0.25,0.2525,0.255,0.2575,0.26,0.2625,0.265,0.2675,0.27,0.2725,0.275,
0.2775,0.28,0.2825,0.285,0.2875,0.29,0.2925,0.295,0.2975,0.3,0.3025,0.305,
0.3075,0.31,0.3125,0.315,0.3175,0.32,0.3225,0.325,0.3275,0.33,0.3325,0.335,
0.3375,0.34,0.3425,0.345,0.3475,0.35,0.3525,0.355,0.3575,0.36,0.3625,0.365,
0.3675,0.37,0.3725,0.375,0.3775,0.38,0.3825,0.385,0.3875,0.39,0.3925,0.395,
0.3975,0.4,0.4025,0.405,0.4075,0.41,0.4125,0.415,0.4175,0.42,0.4225,0.425,
0.4275,0.43,0.4325,0.435,0.4375,0.44,0.4425,0.445,0.4475,0.45,0.4525,0.455,
0.4575,0.46,0.4625,0.465,0.4675,0.47,0.4725,0.475,0.4775,0.48,0.4825,0.485,
0.4875,0.49,0.4925,0.495,0.4975,0.5,0.5025,0.505,0.5075,0.51,0.5125,0.515,
0.5175,0.52,0.5225,0.525,0.5275,0.53,0.5325,0.535,0.5375,0.54,0.5425,0.545,
0.5475,0.55,0.5525,0.555,0.5575,0.56,0.5625,0.565,0.5675,0.57,0.5725,0.575,
0.5775,0.58,0.5825,0.585,0.5875,0.59,0.5925,0.595,0.5975,0.6,0.6025,0.605,
0.6075,0.61,0.6125,0.615,0.6175,0.62,0.6225,0.625,0.6275,0.63,0.6325,0.635,
0.6375,0.64,0.6425,0.645,0.6475,0.65,0.6525,0.655,0.6575,0.66,0.6625,0.665,
0.6675,0.67,0.6725,0.675,0.6775,0.68,0.6825,0.685,0.6875,0.69,0.6925,0.695,
0.6975,0.7,0.7025,0.705,0.7075,0.71,0.7125,0.715,0.7175,0.72,0.7225,0.725,
0.7275,0.73,0.7325,0.735,0.7375,0.74,0.7425,0.745,0.7475,0.75,0.7525,0.755,
0.7575,0.76,0.7625,0.765,0.7675,0.77,0.7725,0.775,0.7775,0.78,0.7825,0.785,
0.7875,0.79,0.7925,0.795,0.7975,0.8,0.8025,0.805,0.8075,0.81,0.8125,0.815,
0.8175,0.82,0.8225,0.825,0.8275,0.83,0.8325,0.835,0.8375,0.84,0.8425,0.845,
0.8475,0.85,0.8525,0.855,0.8575,0.86,0.8625,0.865,0.8675,0.87,0.8725,0.875,
0.8775,0.88,0.8825,0.885,0.8875,0.89,0.8925,0.895,0.8975,0.9,0.9025,0.905,
0.9075,0.91,0.9125,0.915,0.9175,0.92,0.9225,0.925,0.9275,0.93,0.9325,0.935,
0.9375,0.94,0.9425,0.945,0.9475,0.95,0.9525,0.955,0.9575,0.96,0.9625,0.965,
0.9675,0.97,0.9725,0.975,0.9775,0.98,0.9825,0.985,0.9875,0.99,0.9925,0.995,
0.9975,1.),.UNSPECIFIED.)
GEOMETRIC_REPRESENTATION_ITEM()
RATIONAL_B_SPLINE_SURFACE(((1.,0.923879532511287,1.,0.923879532511287,1.,
0.923879532511287,1.,0.923879532511287,1.,0.923879532511287,1.,0.923879532511287,
1.,0.923879532511287,1.,0.923879532511287,1.,0.923879532511287,1.,0.923879532511287,
1.,0.923879532511287,1.,0.923879532511287,1.,0.923879532511287,1.,0.923879532511287,
1.,0.923879532511287,1.,0.923879532511287,1.,0.923879532511287,1.,0.923879532511287,
1.,0.923879532511287,1.,0.923879532511287,1.,0.923879532511287,1.,0.923879532511287,
1.,0.923879532511287,1.,0.923879532511287,1.,0.923879532511287,1.,0.923879532511287,
1.,0.923879532511287,1.,0.923879532511287,1.,0.923879532511287,1.,0.923879532511287,
1.,0.923879532511287,1.,0.923879532511287,1.,0.923879532511287,1.,0.923879532511287,
1.,0.923879532511287,1.,0.923879532511287,1.,0.923879532511287,1.,0.923879532511287,
1.,0.923879532511287,1.,0.923879532511287,1.,0.923879532511287,1.,0.923879532511287,
1.,0.923879532511287,1.,0.923879532511287,1.,0.923879532511287,1.,0.923879532511287,
1.,0.923879532511287,1.,0.923879532511287,1.,0.923879532511287,1.,0.923879532511287,
1.,0.923879532511287,1.,0.923879532511287,1.,0.923879532511287,1.,0.923879532511287,
1.,0.923879532511287,1.,0.923879532511287,1.,0.923879532511287,1.,0.923879532511287,
1.,0.923879532511287,1.,0.923879532511287,1.,0.923879532511287,1.,0.923879532511287,
1.,0.923879532511287,1.,0.923879532511287,1.,0.923879532511287,1.,0.923879532511287,
1.,0.923879532511287,1.,0.923879532511287,1.,0.923879532511287,1.,0.923879532511287,
1.,0.923879532511287,1.,0.923879532511287,1.,0.923879532511287,1.,0.923879532511287,
1.,0.923879532511287,1.,0.923879532511287,1.,0.923879532511287,1.,0.923879532511287,
1.,0.923879532511287,1.,0.923879532511287,1.,0.923879532511287,1.,0.923879532511287,
1.,0.923879532511287,1.,0.923879532511287,1.,0.923879532511287,1.,0.923879532511287,
1.,0.923879532511287,1.,0.923879532511287,1.,0.923879532511287,1.,0.923879532511287,
1.,0.923879532511287,1.,0.923879532511287,1.,0.923879532511287,1.,0.923879532511287,
1.,0.923879532511287,1.,0.923879532511287,1.,0.923879532511287,1.,0.923879532511287,
1.,0.923879532511287,1.,0.923879532511287,1.,0.923879532511287,1.,0.923879532511287,
1.,0.923879532511287,1.,0.923879532511287,1.,0.923879532511287,1.,0.923879532511287,
1.,0.923879532511287,1.,0.923879532511287,1.,0.923879532511287,1.,0.923879532511287,
1.,0.923879532511287,1.,0.923879532511287,1.,0.923879532511287,1.,0.923879532511287,
1.,0.923879532511287,1.,0.923879532511287,1.,0.923879532511287,1.,0.923879532511287,
1.,0.923879532511287,1.,0.923879532511287,1.,0.923879532511287,1.,0.923879532511287,
1.,0.923879532511287,1.,0.923879532511287,1.,0.923879532511287,1.,0.923879532511287,
1.,0.923879532511287,1.,0.923879532511287,1.,0.923879532511287,1.,0.923879532511287,
1.,0.923879532511287,1.,0.923879532511287,1.,0.923879532511287,1.,0.923879532511287,
1.,0.923879532511287,1.,0.923879532511287,1.,0.923879532511287,1.,0.923879532511287,
1.,0.923879532511287,1.,0.923879532511287,1.,0.923879532511287,1.,0.923879532511287,
1.,0.923879532511287,1.,0.923879532511287,1.,0.923879532511287,1.,0.923879532511287,
1.,0.923879532511287,1.,0.923879532511287,1.,0.923879532511287,1.,0.923879532511287,
1.,0.923879532511287,1.,0.923879532511287,1.,0.923879532511287,1.,0.923879532511287,
1.,0.923879532511287,1.,0.923879532511287,1.,0.923879532511287,1.,0.923879532511287,
1.,0.923879532511287,1.,0.923879532511287,1.,0.923879532511287,1.,0.923879532511287,
1.,0.923879532511287,1.,0.923879532511287,1.,0.923879532511287,1.,0.923879532511287,
1.,0.923879532511287,1.,0.923879532511287,1.,0.923879532511287,1.,0.923879532511287,
1.,0.923879532511287,1.,0.923879532511287,1.,0.923879532511287,1.,0.923879532511287,
1.,0.923879532511287,1.,0.923879532511287,1.,0.923879532511287,1.,0.923879532511287,
1.,0.923879532511287,1.,0.923879532511287,1.,0.923879532511287,1.,0.923879532511287,
1.,0.923879532511287,1.,0.923879532511287,1.,0.923879532511287,1.,0.923879532511287,
1.,0.923879532511287,1.,0.923879532511287,1.,0.923879532511287,1.,0.923879532511287,
1.,0.923879532511287,1.,0.923879532511287,1.,0.923879532511287,1.,0.923879532511287,
1.,0.923879532511287,1.,0.923879532511287,1.,0.923879532511287,1.,0.923879532511287,
1.,0.923879532511287,1.,0.923879532511287,1.,0.923879532511287,1.,0.923879532511287,
1.,0.923879532511287,1.,0.923879532511287,1.,0.923879532511287,1.,0.923879532511287,
1.,0.923879532511287,1.,0.923879532511287,1.,0.923879532511287,1.,0.923879532511287,
1.,0.923879532511287,1.,0.923879532511287,1.,0.923879532511287,1.,0.923879532511287,
1.,0.923879532511287,1.,0.923879532511287,1.,0.923879532511287,1.,0.923879532511287,
1.,0.923879532511287,1.,0.923879532511287,1.,0.923879532511287,1.,0.923879532511287,
1.,0.923879532511287,1.,0.923879532511287,1.,0.923879532511287,1.,0.923879532511287,
1.,0.923879532511287,1.,0.923879532511287,1.,0.923879532511287,1.,0.923879532511287,
1.,0.923879532511287,1.,0.923879532511287,1.,0.923879532511287,1.,0.923879532511287,
1.,0.923879532511287,1.,0.923879532511287,1.,0.923879532511287,1.,0.923879532511287,
1.,0.923879532511287,1.,0.923879532511287,1.,0.923879532511287,1.,0.923879532511287,
1.,0.923879532511287,1.,0.923879532511287,1.,0.923879532511287,1.,0.923879532511287,
1.,0.923879532511287,1.,0.923879532511287,1.,0.923879532511287,1.,0.923879532511287,
1.,0.923879532511287,1.,0.923879532511287,1.,0.923879532511287,1.,0.923879532511287,
1.,0.923879532511287,1.,0.923879532511287,1.,0.923879532511287,1.,0.923879532511287,
1.,0.923879532511287,1.,0.923879532511287,1.,0.923879532511287,1.,0.923879532511287,
1.,0.923879532511287,1.,0.923879532511287,1.,0.923879532511287,1.,0.923879532511287,
1.,0.923879532511287,1.,0.923879532511287,1.,0.923879532511287,1.,0.923879532511287,
1.,0.923879532511287,1.,0.923879532511287,1.,0.923879532511287,1.,0.923879532511287,
1.,0.923879532511287,1.,0.923879532511287,1.,0.923879532511287,1.,0.923879532511287,
1.,0.923879532511287,1.,0.923879532511287,1.,0.923879532511287,1.,0.923879532511287,
1.,0.923879532511287,1.,0.923879532511287,1.,0.923879532511287,1.,0.923879532511287,
1.,0.923879532511287,1.,0.923879532511287,1.,0.923879532511287,1.,0.923879532511287,
1.,0.923879532511287,1.,0.923879532511287,1.,0.923879532511287,1.,0.923879532511287,
1.,0.923879532511287,1.,0.923879532511287,1.,0.923879532511287,1.,0.923879532511287,
1.,0.923879532511287,1.,0.923879532511287,1.,0.923879532511287,1.,0.923879532511287,
1.,0.923879532511287,1.,0.923879532511287,1.,0.923879532511287,1.,0.923879532511287,
1.,0.923879532511287,1.,0.923879532511287,1.,0.923879532511287,1.,0.923879532511287,
1.,0.923879532511287,1.,0.923879532511287,1.,0.923879532511287,1.,0.923879532511287,
1.,0.923879532511287,1.,0.923879532511287,1.,0.923879532511287,1.,0.923879532511287,
1.,0.923879532511287,1.,0.923879532511287,1.,0.923879532511287,1.,0.923879532511287,
1.,0.923879532511287,1.,0.923879532511287,1.,0.923879532511287,1.,0.923879532511287,
1.,0.923879532511287,1.,0.923879532511287,1.,0.923879532511287,1.,0.923879532511287,
1.,0.923879532511287,1.,0.923879532511287,1.,0.923879532511287,1.,0.923879532511287,
1.,0.923879532511287,1.,0.923879532511287,1.,0.923879532511287,1.,0.923879532511287,
1.,0.923879532511287,1.,0.923879532511287,1.,0.923879532511287,1.,0.923879532511287,
1.,0.923879532511287,1.,0.923879532511287,1.,0.923879532511287,1.,0.923879532511287,
1.,0.923879532511287,1.,0.923879532511287,1.,0.923879532511287,1.,0.923879532511287,
1.,0.923879532511287,1.,0.923879532511287,1.,0.923879532511287,1.,0.923879532511287,
1.,0.923879532511287,1.,0.923879532511287,1.,0.923879532511287,1.,0.923879532511287,
1.,0.923879532511287,1.,0.923879532511287,1.,0.923879532511287,1.,0.923879532511287,
1.,0.923879532511287,1.,0.923879532511287,1.,0.923879532511287,1.,0.923879532511287,
1.,0.923879532511287,1.,0.923879532511287,1.,0.923879532511287,1.,0.923879532511287,
1.,0.923879532511287,1.,0.923879532511287,1.,0.923879532511287,1.,0.923879532511287,
1.,0.923879532511287,1.,0.923879532511287,1.,0.923879532511287,1.,0.923879532511287,
1.,0.923879532511287,1.,0.923879532511287,1.,0.923879532511287,1.,0.923879532511287,
1.,0.923879532511287,1.,0.923879532511287,1.,0.923879532511287,1.,0.923879532511287,
1.,0.923879532511287,1.,0.923879532511287,1.,0.923879532511287,1.,0.923879532511287,
1.,0.923879532511287,1.,0.923879532511287,1.,0.923879532511287,1.,0.923879532511287,
1.,0.923879532511287,1.,0.923879532511287,1.,0.923879532511287,1.,0.923879532511287,
1.,0.923879532511287,1.,0.923879532511287,1.),(1.,0.923879532511287,1.,
0.923879532511287,1.,0.923879532511287,1.,0.923879532511287,1.,0.923879532511287,
1.,0.923879532511287,1.,0.923879532511287,1.,0.923879532511287,1.,0.923879532511287,
1.,0.923879532511287,1.,0.923879532511287,1.,0.923879532511287,1.,0.923879532511287,
1.,0.923879532511287,1.,0.923879532511287,1.,0.923879532511287,1.,0.923879532511287,
1.,0.923879532511287,1.,0.923879532511287,1.,0.923879532511287,1.,0.923879532511287,
1.,0.923879532511287,1.,0.923879532511287,1.,0.923879532511287,1.,0.923879532511287,
1.,0.923879532511287,1.,0.923879532511287,1.,0.923879532511287,1.,0.923879532511287,
1.,0.923879532511287,1.,0.923879532511287,1.,0.923879532511287,1.,0.923879532511287,
1.,0.923879532511287,1.,0.923879532511287,1.,0.923879532511287,1.,0.923879532511287,
1.,0.923879532511287,1.,0.923879532511287,1.,0.923879532511287,1.,0.923879532511287,
1.,0.923879532511287,1.,0.923879532511287,1.,0.923879532511287,1.,0.923879532511287,
1.,0.923879532511287,1.,0.923879532511287,1.,0.923879532511287,1.,0.923879532511287,
1.,0.923879532511287,1.,0.923879532511287,1.,0.923879532511287,1.,0.923879532511287,
1.,0.923879532511287,1.,0.923879532511287,1.,0.923879532511287,1.,0.923879532511287,
1.,0.923879532511287,1.,0.923879532511287,1.,0.923879532511287,1.,0.923879532511287,
1.,0.923879532511287,1.,0.923879532511287,1.,0.923879532511287,1.,0.923879532511287,
1.,0.923879532511287,1.,0.923879532511287,1.,0.923879532511287,1.,0.923879532511287,
1.,0.923879532511287,1.,0.923879532511287,1.,0.923879532511287,1.,0.923879532511287,
1.,0.923879532511287,1.,0.923879532511287,1.,0.923879532511287,1.,0.923879532511287,
1.,0.923879532511287,1.,0.923879532511287,1.,0.923879532511287,1.,0.923879532511287,
1.,0.923879532511287,1.,0.923879532511287,1.,0.923879532511287,1.,0.923879532511287,
1.,0.923879532511287,1.,0.923879532511287,1.,0.923879532511287,1.,0.923879532511287,
1.,0.923879532511287,1.,0.923879532511287,1.,0.923879532511287,1.,0.923879532511287,
1.,0.923879532511287,1.,0.923879532511287,1.,0.923879532511287,1.,0.923879532511287,
1.,0.923879532511287,1.,0.923879532511287,1.,0.923879532511287,1.,0.923879532511287,
1.,0.923879532511287,1.,0.923879532511287,1.,0.923879532511287,1.,0.923879532511287,
1.,0.923879532511287,1.,0.923879532511287,1.,0.923879532511287,1.,0.923879532511287,
1.,0.923879532511287,1.,0.923879532511287,1.,0.923879532511287,1.,0.923879532511287,
1.,0.923879532511287,1.,0.923879532511287,1.,0.923879532511287,1.,0.923879532511287,
1.,0.923879532511287,1.,0.923879532511287,1.,0.923879532511287,1.,0.923879532511287,
1.,0.923879532511287,1.,0.923879532511287,1.,0.923879532511287,1.,0.923879532511287,
1.,0.923879532511287,1.,0.923879532511287,1.,0.923879532511287,1.,0.923879532511287,
1.,0.923879532511287,1.,0.923879532511287,1.,0.923879532511287,1.,0.923879532511287,
1.,0.923879532511287,1.,0.923879532511287,1.,0.923879532511287,1.,0.923879532511287,
1.,0.923879532511287,1.,0.923879532511287,1.,0.923879532511287,1.,0.923879532511287,
1.,0.923879532511287,1.,0.923879532511287,1.,0.923879532511287,1.,0.923879532511287,
1.,0.923879532511287,1.,0.923879532511287,1.,0.923879532511287,1.,0.923879532511287,
1.,0.923879532511287,1.,0.923879532511287,1.,0.923879532511287,1.,0.923879532511287,
1.,0.923879532511287,1.,0.923879532511287,1.,0.923879532511287,1.,0.923879532511287,
1.,0.923879532511287,1.,0.923879532511287,1.,0.923879532511287,1.,0.923879532511287,
1.,0.923879532511287,1.,0.923879532511287,1.,0.923879532511287,1.,0.923879532511287,
1.,0.923879532511287,1.,0.923879532511287,1.,0.923879532511287,1.,0.923879532511287,
1.,0.923879532511287,1.,0.923879532511287,1.,0.923879532511287,1.,0.923879532511287,
1.,0.923879532511287,1.,0.923879532511287,1.,0.923879532511287,1.,0.923879532511287,
1.,0.923879532511287,1.,0.923879532511287,1.,0.923879532511287,1.,0.923879532511287,
1.,0.923879532511287,1.,0.923879532511287,1.,0.923879532511287,1.,0.923879532511287,
1.,0.923879532511287,1.,0.923879532511287,1.,0.923879532511287,1.,0.923879532511287,
1.,0.923879532511287,1.,0.923879532511287,1.,0.923879532511287,1.,0.923879532511287,
1.,0.923879532511287,1.,0.923879532511287,1.,0.923879532511287,1.,0.923879532511287,
1.,0.923879532511287,1.,0.923879532511287,1.,0.923879532511287,1.,0.923879532511287,
1.,0.923879532511287,1.,0.923879532511287,1.,0.923879532511287,1.,0.923879532511287,
1.,0.923879532511287,1.,0.923879532511287,1.,0.923879532511287,1.,0.923879532511287,
1.,0.923879532511287,1.,0.923879532511287,1.,0.923879532511287,1.,0.923879532511287,
1.,0.923879532511287,1.,0.923879532511287,1.,0.923879532511287,1.,0.923879532511287,
1.,0.923879532511287,1.,0.923879532511287,1.,0.923879532511287,1.,0.923879532511287,
1.,0.923879532511287,1.,0.923879532511287,1.,0.923879532511287,1.,0.923879532511287,
1.,0.923879532511287,1.,0.923879532511287,1.,0.923879532511287,1.,0.923879532511287,
1.,0.923879532511287,1.,0.923879532511287,1.,0.923879532511287,1.,0.923879532511287,
1.,0.923879532511287,1.,0.923879532511287,1.,0.923879532511287,1.,0.923879532511287,
1.,0.923879532511287,1.,0.923879532511287,1.,0.923879532511287,1.,0.923879532511287,
1.,0.923879532511287,1.,0.923879532511287,1.,0.923879532511287,1.,0.923879532511287,
1.,0.923879532511287,1.,0.923879532511287,1.,0.923879532511287,1.,0.923879532511287,
1.,0.923879532511287,1.,0.923879532511287,1.,0.923879532511287,1.,0.923879532511287,
1.,0.923879532511287,1.,0.923879532511287,1.,0.923879532511287,1.,0.923879532511287,
1.,0.923879532511287,1.,0.923879532511287,1.,0.923879532511287,1.,0.923879532511287,
1.,0.923879532511287,1.,0.923879532511287,1.,0.923879532511287,1.,0.923879532511287,
1.,0.923879532511287,1.,0.923879532511287,1.,0.923879532511287,1.,0.923879532511287,
1.,0.923879532511287,1.,0.923879532511287,1.,0.923879532511287,1.,0.923879532511287,
1.,0.923879532511287,1.,0.923879532511287,1.,0.923879532511287,1.,0.923879532511287,
1.,0.923879532511287,1.,0.923879532511287,1.,0.923879532511287,1.,0.923879532511287,
1.,0.923879532511287,1.,0.923879532511287,1.,0.923879532511287,1.,0.923879532511287,
1.,0.923879532511287,1.,0.923879532511287,1.,0.923879532511287,1.,0.923879532511287,
1.,0.923879532511287,1.,0.923879532511287,1.,0.923879532511287,1.,0.923879532511287,
1.,0.923879532511287,1.,0.923879532511287,1.,0.923879532511287,1.,0.923879532511287,
1.,0.923879532511287,1.,0.923879532511287,1.,0.923879532511287,1.,0.923879532511287,
1.,0.923879532511287,1.,0.923879532511287,1.,0.923879532511287,1.,0.923879532511287,
1.,0.923879532511287,1.,0.923879532511287,1.,0.923879532511287,1.,0.923879532511287,
1.,0.923879532511287,1.,0.923879532511287,1.,0.923879532511287,1.,0.923879532511287,
1.,0.923879532511287,1.,0.923879532511287,1.,0.923879532511287,1.,0.923879532511287,
1.,0.923879532511287,1.,0.923879532511287,1.,0.923879532511287,1.,0.923879532511287,
1.,0.923879532511287,1.,0.923879532511287,1.,0.923879532511287,1.,0.923879532511287,
1.,0.923879532511287,1.,0.923879532511287,1.,0.923879532511287,1.,0.923879532511287,
1.,0.923879532511287,1.,0.923879532511287,1.,0.923879532511287,1.,0.923879532511287,
1.,0.923879532511287,1.,0.923879532511287,1.,0.923879532511287,1.,0.923879532511287,
1.,0.923879532511287,1.,0.923879532511287,1.,0.923879532511287,1.,0.923879532511287,
1.,0.923879532511287,1.,0.923879532511287,1.,0.923879532511287,1.,0.923879532511287,
1.,0.923879532511287,1.,0.923879532511287,1.,0.923879532511287,1.,0.923879532511287,
1.,0.923879532511287,1.,0.923879532511287,1.,0.923879532511287,1.,0.923879532511287,
1.,0.923879532511287,1.,0.923879532511287,1.,0.923879532511287,1.,0.923879532511287,
1.,0.923879532511287,1.,0.923879532511287,1.,0.923879532511287,1.,0.923879532511287,
1.,0.923879532511287,1.,0.923879532511287,1.,0.923879532511287,1.,0.923879532511287,
1.,0.923879532511287,1.,0.923879532511287,1.,0.923879532511287,1.,0.923879532511287,
1.,0.923879532511287,1.,0.923879532511287,1.,0.923879532511287,1.,0.923879532511287,
1.,0.923879532511287,1.,0.923879532511287,1.,0.923879532511287,1.,0.923879532511287,
1.,0.923879532511287,1.,0.923879532511287,1.,0.923879532511287,1.,0.923879532511287,
1.,0.923879532511287,1.,0.923879532511287,1.,0.923879532511287,1.,0.923879532511287,
1.,0.923879532511287,1.,0.923879532511287,1.,0.923879532511287,1.,0.923879532511287,
1.,0.923879532511287,1.,0.923879532511287,1.,0.923879532511287,1.,0.923879532511287,
1.,0.923879532511287,1.,0.923879532511287,1.,0.923879532511287,1.,0.923879532511287,
1.,0.923879532511287,1.,0.923879532511287,1.,0.923879532511287,1.)))
REPRESENTATION_ITEM('')
SURFACE()
);
#71=(
BOUNDED_SURFACE()
B_SPLINE_SURFACE(1,2,((#12578,#12579,#12580,#12581,#12582,#12583,#12584,
#12585,#12586,#12587,#12588,#12589,#12590,#12591,#12592,#12593,#12594,#12595,
#12596,#12597,#12598,#12599,#12600,#12601,#12602,#12603,#12604,#12605,#12606,
#12607,#12608,#12609,#12610,#12611,#12612,#12613,#12614,#12615,#12616,#12617,
#12618,#12619,#12620,#12621,#12622,#12623,#12624,#12625,#12626,#12627,#12628,
#12629,#12630,#12631,#12632,#12633,#12634,#12635,#12636,#12637,#12638,#12639,
#12640,#12641,#12642,#12643,#12644,#12645,#12646,#12647,#12648,#12649,#12650,
#12651,#12652,#12653,#12654,#12655,#12656,#12657,#12658,#12659,#12660,#12661,
#12662,#12663,#12664,#12665,#12666,#12667,#12668,#12669,#12670,#12671,#12672,
#12673,#12674,#12675,#12676,#12677,#12678,#12679,#12680,#12681,#12682,#12683,
#12684,#12685,#12686,#12687,#12688,#12689,#12690,#12691,#12692,#12693,#12694,
#12695,#12696,#12697,#12698),(#12699,#12700,#12701,#12702,#12703,#12704,
#12705,#12706,#12707,#12708,#12709,#12710,#12711,#12712,#12713,#12714,#12715,
#12716,#12717,#12718,#12719,#12720,#12721,#12722,#12723,#12724,#12725,#12726,
#12727,#12728,#12729,#12730,#12731,#12732,#12733,#12734,#12735,#12736,#12737,
#12738,#12739,#12740,#12741,#12742,#12743,#12744,#12745,#12746,#12747,#12748,
#12749,#12750,#12751,#12752,#12753,#12754,#12755,#12756,#12757,#12758,#12759,
#12760,#12761,#12762,#12763,#12764,#12765,#12766,#12767,#12768,#12769,#12770,
#12771,#12772,#12773,#12774,#12775,#12776,#12777,#12778,#12779,#12780,#12781,
#12782,#12783,#12784,#12785,#12786,#12787,#12788,#12789,#12790,#12791,#12792,
#12793,#12794,#12795,#12796,#12797,#12798,#12799,#12800,#12801,#12802,#12803,
#12804,#12805,#12806,#12807,#12808,#12809,#12810,#12811,#12812,#12813,#12814,
#12815,#12816,#12817,#12818,#12819)),.UNSPECIFIED.,.F.,.F.,.F.)
B_SPLINE_SURFACE_WITH_KNOTS((2,2),(3,2,2,2,2,2,2,2,2,2,2,2,2,2,2,2,2,2,
2,2,2,2,2,2,2,2,2,2,2,2,2,2,2,2,2,2,2,2,2,2,2,2,2,2,2,2,2,2,2,2,2,2,2,2,
2,2,2,2,2,2,3),(0.,1.),(0.,0.0166666666666667,0.0333333333333333,0.05,0.0666666666666667,
0.0833333333333333,0.1,0.116666666666667,0.133333333333333,0.15,0.166666666666667,
0.183333333333333,0.2,0.216666666666667,0.233333333333333,0.25,0.266666666666667,
0.283333333333333,0.3,0.316666666666667,0.333333333333333,0.35,0.366666666666667,
0.383333333333333,0.4,0.416666666666667,0.433333333333333,0.45,0.466666666666667,
0.483333333333333,0.5,0.516666666666667,0.533333333333333,0.55,0.566666666666667,
0.583333333333333,0.6,0.616666666666667,0.633333333333333,0.65,0.666666666666667,
0.683333333333333,0.7,0.716666666666667,0.733333333333333,0.75,0.766666666666667,
0.783333333333333,0.8,0.816666666666667,0.833333333333333,0.85,0.866666666666667,
0.883333333333333,0.9,0.916666666666667,0.933333333333333,0.95,0.966666666666667,
0.983333333333333,1.),.UNSPECIFIED.)
GEOMETRIC_REPRESENTATION_ITEM()
RATIONAL_B_SPLINE_SURFACE(((1.,0.987688340595138,1.,0.987688340595138,1.,
0.987688340595138,1.,0.987688340595138,1.,0.987688340595138,1.,0.987688340595138,
1.,0.987688340595138,1.,0.987688340595138,1.,0.987688340595138,1.,0.987688340595138,
1.,0.987688340595138,1.,0.987688340595138,1.,0.987688340595138,1.,0.987688340595138,
1.,0.987688340595138,1.,0.987688340595138,1.,0.987688340595138,1.,0.987688340595138,
1.,0.987688340595138,1.,0.987688340595138,1.,0.987688340595138,1.,0.987688340595138,
1.,0.987688340595138,1.,0.987688340595138,1.,0.987688340595138,1.,0.987688340595138,
1.,0.987688340595138,1.,0.987688340595138,1.,0.987688340595138,1.,0.987688340595138,
1.,0.987688340595138,1.,0.987688340595138,1.,0.987688340595138,1.,0.987688340595138,
1.,0.987688340595138,1.,0.987688340595138,1.,0.987688340595138,1.,0.987688340595138,
1.,0.987688340595138,1.,0.987688340595138,1.,0.987688340595138,1.,0.987688340595138,
1.,0.987688340595138,1.,0.987688340595138,1.,0.987688340595138,1.,0.987688340595138,
1.,0.987688340595138,1.,0.987688340595138,1.,0.987688340595138,1.,0.987688340595138,
1.,0.987688340595138,1.,0.987688340595138,1.,0.987688340595138,1.,0.987688340595138,
1.,0.987688340595138,1.,0.987688340595138,1.,0.987688340595138,1.,0.987688340595138,
1.,0.987688340595138,1.,0.987688340595138,1.),(1.,0.987688340595138,1.,
0.987688340595138,1.,0.987688340595138,1.,0.987688340595138,1.,0.987688340595138,
1.,0.987688340595138,1.,0.987688340595138,1.,0.987688340595138,1.,0.987688340595138,
1.,0.987688340595138,1.,0.987688340595138,1.,0.987688340595138,1.,0.987688340595138,
1.,0.987688340595138,1.,0.987688340595138,1.,0.987688340595138,1.,0.987688340595138,
1.,0.987688340595138,1.,0.987688340595138,1.,0.987688340595138,1.,0.987688340595138,
1.,0.987688340595138,1.,0.987688340595138,1.,0.987688340595138,1.,0.987688340595138,
1.,0.987688340595138,1.,0.987688340595138,1.,0.987688340595138,1.,0.987688340595138,
1.,0.987688340595138,1.,0.987688340595138,1.,0.987688340595138,1.,0.987688340595138,
1.,0.987688340595138,1.,0.987688340595138,1.,0.987688340595138,1.,0.987688340595138,
1.,0.987688340595138,1.,0.987688340595138,1.,0.987688340595138,1.,0.987688340595138,
1.,0.987688340595138,1.,0.987688340595138,1.,0.987688340595138,1.,0.987688340595138,
1.,0.987688340595138,1.,0.987688340595138,1.,0.987688340595138,1.,0.987688340595138,
1.,0.987688340595138,1.,0.987688340595138,1.,0.987688340595138,1.,0.987688340595138,
1.,0.987688340595138,1.,0.987688340595138,1.,0.987688340595138,1.,0.987688340595138,
1.,0.987688340595138,1.,0.987688340595138,1.,0.987688340595138,1.)))
REPRESENTATION_ITEM('')
SURFACE()
);
#72=(
BOUNDED_SURFACE()
B_SPLINE_SURFACE(1,2,((#12941,#12942,#12943,#12944,#12945,#12946,#12947,
#12948,#12949,#12950,#12951,#12952,#12953,#12954,#12955,#12956,#12957,#12958,
#12959,#12960,#12961,#12962,#12963,#12964,#12965,#12966,#12967,#12968,#12969,
#12970,#12971,#12972,#12973,#12974,#12975,#12976,#12977,#12978,#12979,#12980,
#12981,#12982,#12983,#12984,#12985,#12986,#12987,#12988,#12989,#12990,#12991,
#12992,#12993,#12994,#12995,#12996,#12997,#12998,#12999,#13000,#13001,#13002,
#13003,#13004,#13005,#13006,#13007,#13008,#13009,#13010,#13011,#13012,#13013,
#13014,#13015,#13016,#13017,#13018,#13019,#13020,#13021,#13022,#13023,#13024,
#13025,#13026,#13027,#13028,#13029,#13030,#13031,#13032,#13033,#13034,#13035,
#13036,#13037,#13038,#13039,#13040,#13041,#13042,#13043,#13044,#13045,#13046,
#13047,#13048,#13049,#13050,#13051,#13052,#13053,#13054,#13055,#13056,#13057,
#13058,#13059,#13060,#13061),(#13062,#13063,#13064,#13065,#13066,#13067,
#13068,#13069,#13070,#13071,#13072,#13073,#13074,#13075,#13076,#13077,#13078,
#13079,#13080,#13081,#13082,#13083,#13084,#13085,#13086,#13087,#13088,#13089,
#13090,#13091,#13092,#13093,#13094,#13095,#13096,#13097,#13098,#13099,#13100,
#13101,#13102,#13103,#13104,#13105,#13106,#13107,#13108,#13109,#13110,#13111,
#13112,#13113,#13114,#13115,#13116,#13117,#13118,#13119,#13120,#13121,#13122,
#13123,#13124,#13125,#13126,#13127,#13128,#13129,#13130,#13131,#13132,#13133,
#13134,#13135,#13136,#13137,#13138,#13139,#13140,#13141,#13142,#13143,#13144,
#13145,#13146,#13147,#13148,#13149,#13150,#13151,#13152,#13153,#13154,#13155,
#13156,#13157,#13158,#13159,#13160,#13161,#13162,#13163,#13164,#13165,#13166,
#13167,#13168,#13169,#13170,#13171,#13172,#13173,#13174,#13175,#13176,#13177,
#13178,#13179,#13180,#13181,#13182)),.UNSPECIFIED.,.F.,.F.,.F.)
B_SPLINE_SURFACE_WITH_KNOTS((2,2),(3,2,2,2,2,2,2,2,2,2,2,2,2,2,2,2,2,2,
2,2,2,2,2,2,2,2,2,2,2,2,2,2,2,2,2,2,2,2,2,2,2,2,2,2,2,2,2,2,2,2,2,2,2,2,
2,2,2,2,2,2,3),(0.,1.),(0.,0.0166666666666667,0.0333333333333333,0.05,0.0666666666666667,
0.0833333333333333,0.1,0.116666666666667,0.133333333333333,0.15,0.166666666666667,
0.183333333333333,0.2,0.216666666666667,0.233333333333333,0.25,0.266666666666667,
0.283333333333333,0.3,0.316666666666667,0.333333333333333,0.35,0.366666666666667,
0.383333333333333,0.4,0.416666666666667,0.433333333333333,0.45,0.466666666666667,
0.483333333333333,0.5,0.516666666666667,0.533333333333333,0.55,0.566666666666667,
0.583333333333333,0.6,0.616666666666667,0.633333333333333,0.65,0.666666666666667,
0.683333333333333,0.7,0.716666666666667,0.733333333333333,0.75,0.766666666666667,
0.783333333333333,0.8,0.816666666666667,0.833333333333333,0.85,0.866666666666667,
0.883333333333333,0.9,0.916666666666667,0.933333333333333,0.95,0.966666666666667,
0.983333333333333,1.),.UNSPECIFIED.)
GEOMETRIC_REPRESENTATION_ITEM()
RATIONAL_B_SPLINE_SURFACE(((1.,0.987688340595138,1.,0.987688340595138,1.,
0.987688340595138,1.,0.987688340595138,1.,0.987688340595138,1.,0.987688340595138,
1.,0.987688340595138,1.,0.987688340595138,1.,0.987688340595138,1.,0.987688340595138,
1.,0.987688340595138,1.,0.987688340595138,1.,0.987688340595138,1.,0.987688340595138,
1.,0.987688340595138,1.,0.987688340595138,1.,0.987688340595138,1.,0.987688340595138,
1.,0.987688340595138,1.,0.987688340595138,1.,0.987688340595138,1.,0.987688340595138,
1.,0.987688340595138,1.,0.987688340595138,1.,0.987688340595138,1.,0.987688340595138,
1.,0.987688340595138,1.,0.987688340595138,1.,0.987688340595138,1.,0.987688340595138,
1.,0.987688340595138,1.,0.987688340595138,1.,0.987688340595138,1.,0.987688340595138,
1.,0.987688340595138,1.,0.987688340595138,1.,0.987688340595138,1.,0.987688340595138,
1.,0.987688340595138,1.,0.987688340595138,1.,0.987688340595138,1.,0.987688340595138,
1.,0.987688340595138,1.,0.987688340595138,1.,0.987688340595138,1.,0.987688340595138,
1.,0.987688340595138,1.,0.987688340595138,1.,0.987688340595138,1.,0.987688340595138,
1.,0.987688340595138,1.,0.987688340595138,1.,0.987688340595138,1.,0.987688340595138,
1.,0.987688340595138,1.,0.987688340595138,1.,0.987688340595138,1.,0.987688340595138,
1.,0.987688340595138,1.,0.987688340595138,1.),(1.,0.987688340595138,1.,
0.987688340595138,1.,0.987688340595138,1.,0.987688340595138,1.,0.987688340595138,
1.,0.987688340595138,1.,0.987688340595138,1.,0.987688340595138,1.,0.987688340595138,
1.,0.987688340595138,1.,0.987688340595138,1.,0.987688340595138,1.,0.987688340595138,
1.,0.987688340595138,1.,0.987688340595138,1.,0.987688340595138,1.,0.987688340595138,
1.,0.987688340595138,1.,0.987688340595138,1.,0.987688340595138,1.,0.987688340595138,
1.,0.987688340595138,1.,0.987688340595138,1.,0.987688340595138,1.,0.987688340595138,
1.,0.987688340595138,1.,0.987688340595138,1.,0.987688340595138,1.,0.987688340595138,
1.,0.987688340595138,1.,0.987688340595138,1.,0.987688340595138,1.,0.987688340595138,
1.,0.987688340595138,1.,0.987688340595138,1.,0.987688340595138,1.,0.987688340595138,
1.,0.987688340595138,1.,0.987688340595138,1.,0.987688340595138,1.,0.987688340595138,
1.,0.987688340595138,1.,0.987688340595138,1.,0.987688340595138,1.,0.987688340595138,
1.,0.987688340595138,1.,0.987688340595138,1.,0.987688340595138,1.,0.987688340595138,
1.,0.987688340595138,1.,0.987688340595138,1.,0.987688340595138,1.,0.987688340595138,
1.,0.987688340595138,1.,0.987688340595138,1.,0.987688340595138,1.,0.987688340595138,
1.,0.987688340595138,1.,0.987688340595138,1.,0.987688340595138,1.)))
REPRESENTATION_ITEM('')
SURFACE()
);
#73=(
BOUNDED_SURFACE()
B_SPLINE_SURFACE(1,2,((#13304,#13305,#13306,#13307,#13308,#13309,#13310,
#13311,#13312,#13313,#13314,#13315,#13316,#13317,#13318,#13319,#13320,#13321,
#13322,#13323,#13324,#13325,#13326,#13327,#13328,#13329,#13330,#13331,#13332,
#13333,#13334,#13335,#13336,#13337,#13338,#13339,#13340,#13341,#13342,#13343,
#13344,#13345,#13346,#13347,#13348,#13349,#13350,#13351,#13352,#13353,#13354,
#13355,#13356,#13357,#13358,#13359,#13360,#13361,#13362,#13363,#13364,#13365,
#13366,#13367,#13368,#13369,#13370,#13371,#13372,#13373,#13374,#13375,#13376,
#13377,#13378,#13379,#13380,#13381,#13382,#13383,#13384,#13385,#13386,#13387,
#13388,#13389,#13390,#13391,#13392,#13393,#13394,#13395,#13396,#13397,#13398,
#13399,#13400,#13401,#13402,#13403,#13404,#13405,#13406,#13407,#13408,#13409,
#13410,#13411,#13412,#13413,#13414,#13415,#13416,#13417,#13418,#13419,#13420,
#13421,#13422,#13423,#13424),(#13425,#13426,#13427,#13428,#13429,#13430,
#13431,#13432,#13433,#13434,#13435,#13436,#13437,#13438,#13439,#13440,#13441,
#13442,#13443,#13444,#13445,#13446,#13447,#13448,#13449,#13450,#13451,#13452,
#13453,#13454,#13455,#13456,#13457,#13458,#13459,#13460,#13461,#13462,#13463,
#13464,#13465,#13466,#13467,#13468,#13469,#13470,#13471,#13472,#13473,#13474,
#13475,#13476,#13477,#13478,#13479,#13480,#13481,#13482,#13483,#13484,#13485,
#13486,#13487,#13488,#13489,#13490,#13491,#13492,#13493,#13494,#13495,#13496,
#13497,#13498,#13499,#13500,#13501,#13502,#13503,#13504,#13505,#13506,#13507,
#13508,#13509,#13510,#13511,#13512,#13513,#13514,#13515,#13516,#13517,#13518,
#13519,#13520,#13521,#13522,#13523,#13524,#13525,#13526,#13527,#13528,#13529,
#13530,#13531,#13532,#13533,#13534,#13535,#13536,#13537,#13538,#13539,#13540,
#13541,#13542,#13543,#13544,#13545)),.UNSPECIFIED.,.F.,.F.,.F.)
B_SPLINE_SURFACE_WITH_KNOTS((2,2),(3,2,2,2,2,2,2,2,2,2,2,2,2,2,2,2,2,2,
2,2,2,2,2,2,2,2,2,2,2,2,2,2,2,2,2,2,2,2,2,2,2,2,2,2,2,2,2,2,2,2,2,2,2,2,
2,2,2,2,2,2,3),(0.,1.),(0.,0.0166666666666667,0.0333333333333333,0.05,0.0666666666666667,
0.0833333333333333,0.1,0.116666666666667,0.133333333333333,0.15,0.166666666666667,
0.183333333333333,0.2,0.216666666666667,0.233333333333333,0.25,0.266666666666667,
0.283333333333333,0.3,0.316666666666667,0.333333333333333,0.35,0.366666666666667,
0.383333333333333,0.4,0.416666666666667,0.433333333333333,0.45,0.466666666666667,
0.483333333333333,0.5,0.516666666666667,0.533333333333333,0.55,0.566666666666667,
0.583333333333333,0.6,0.616666666666667,0.633333333333333,0.65,0.666666666666667,
0.683333333333333,0.7,0.716666666666667,0.733333333333333,0.75,0.766666666666667,
0.783333333333333,0.8,0.816666666666667,0.833333333333333,0.85,0.866666666666667,
0.883333333333333,0.9,0.916666666666667,0.933333333333333,0.95,0.966666666666667,
0.983333333333333,1.),.UNSPECIFIED.)
GEOMETRIC_REPRESENTATION_ITEM()
RATIONAL_B_SPLINE_SURFACE(((1.,0.987688340595138,1.,0.987688340595138,1.,
0.987688340595138,1.,0.987688340595138,1.,0.987688340595138,1.,0.987688340595138,
1.,0.987688340595138,1.,0.987688340595138,1.,0.987688340595138,1.,0.987688340595138,
1.,0.987688340595138,1.,0.987688340595138,1.,0.987688340595138,1.,0.987688340595138,
1.,0.987688340595138,1.,0.987688340595138,1.,0.987688340595138,1.,0.987688340595138,
1.,0.987688340595138,1.,0.987688340595138,1.,0.987688340595138,1.,0.987688340595138,
1.,0.987688340595138,1.,0.987688340595138,1.,0.987688340595138,1.,0.987688340595138,
1.,0.987688340595138,1.,0.987688340595138,1.,0.987688340595138,1.,0.987688340595138,
1.,0.987688340595138,1.,0.987688340595138,1.,0.987688340595138,1.,0.987688340595138,
1.,0.987688340595138,1.,0.987688340595138,1.,0.987688340595138,1.,0.987688340595138,
1.,0.987688340595138,1.,0.987688340595138,1.,0.987688340595138,1.,0.987688340595138,
1.,0.987688340595138,1.,0.987688340595138,1.,0.987688340595138,1.,0.987688340595138,
1.,0.987688340595138,1.,0.987688340595138,1.,0.987688340595138,1.,0.987688340595138,
1.,0.987688340595138,1.,0.987688340595138,1.,0.987688340595138,1.,0.987688340595138,
1.,0.987688340595138,1.,0.987688340595138,1.,0.987688340595138,1.,0.987688340595138,
1.,0.987688340595138,1.,0.987688340595138,1.),(1.,0.987688340595138,1.,
0.987688340595138,1.,0.987688340595138,1.,0.987688340595138,1.,0.987688340595138,
1.,0.987688340595138,1.,0.987688340595138,1.,0.987688340595138,1.,0.987688340595138,
1.,0.987688340595138,1.,0.987688340595138,1.,0.987688340595138,1.,0.987688340595138,
1.,0.987688340595138,1.,0.987688340595138,1.,0.987688340595138,1.,0.987688340595138,
1.,0.987688340595138,1.,0.987688340595138,1.,0.987688340595138,1.,0.987688340595138,
1.,0.987688340595138,1.,0.987688340595138,1.,0.987688340595138,1.,0.987688340595138,
1.,0.987688340595138,1.,0.987688340595138,1.,0.987688340595138,1.,0.987688340595138,
1.,0.987688340595138,1.,0.987688340595138,1.,0.987688340595138,1.,0.987688340595138,
1.,0.987688340595138,1.,0.987688340595138,1.,0.987688340595138,1.,0.987688340595138,
1.,0.987688340595138,1.,0.987688340595138,1.,0.987688340595138,1.,0.987688340595138,
1.,0.987688340595138,1.,0.987688340595138,1.,0.987688340595138,1.,0.987688340595138,
1.,0.987688340595138,1.,0.987688340595138,1.,0.987688340595138,1.,0.987688340595138,
1.,0.987688340595138,1.,0.987688340595138,1.,0.987688340595138,1.,0.987688340595138,
1.,0.987688340595138,1.,0.987688340595138,1.,0.987688340595138,1.,0.987688340595138,
1.,0.987688340595138,1.,0.987688340595138,1.,0.987688340595138,1.)))
REPRESENTATION_ITEM('')
SURFACE()
);
#74=CONICAL_SURFACE('',#3154,118.168461709225,0.436332312998584);
#75=CONICAL_SURFACE('',#3165,114.797295826488,0.139626340159547);
#76=CONICAL_SURFACE('',#3166,120.5,0.523598775598293);
#77=CONICAL_SURFACE('',#3178,15.,0.785398163397452);
#78=CONICAL_SURFACE('',#3208,52.,0.463647609000806);
#79=CONICAL_SURFACE('',#3210,200.,0.463647609000806);
#80=PLANE('',#3146);
#81=PLANE('',#3149);
#82=PLANE('',#3152);
#83=PLANE('',#3155);
#84=PLANE('',#3156);
#85=PLANE('',#3161);
#86=PLANE('',#3164);
#87=PLANE('',#3168);
#88=PLANE('',#3173);
#89=PLANE('',#3177);
#90=PLANE('',#3185);
#91=PLANE('',#3188);
#92=PLANE('',#3195);
#93=PLANE('',#3199);
#94=PLANE('',#3203);
#95=PLANE('',#3205);
#96=PLANE('',#3217);
#97=PLANE('',#3221);
#98=PLANE('',#3222);
#99=PLANE('',#3224);
#100=PLANE('',#3239);
#101=PLANE('',#3247);
#102=PLANE('',#3248);
#103=PLANE('',#3251);
#104=PLANE('',#3260);
#105=PLANE('',#3261);
#106=PLANE('',#3262);
#107=PLANE('',#3266);
#108=PLANE('',#3267);
#109=PLANE('',#3268);
#110=PLANE('',#3269);
#111=PLANE('',#3270);
#112=FACE_BOUND('',#477,.T.);
#113=FACE_BOUND('',#478,.T.);
#114=FACE_BOUND('',#481,.T.);
#115=FACE_BOUND('',#483,.T.);
#116=FACE_BOUND('',#485,.T.);
#117=FACE_BOUND('',#502,.T.);
#118=FACE_BOUND('',#508,.T.);
#119=FACE_BOUND('',#510,.T.);
#120=FACE_BOUND('',#512,.T.);
#121=FACE_BOUND('',#514,.T.);
#122=FACE_BOUND('',#517,.T.);
#123=FACE_BOUND('',#520,.T.);
#124=FACE_BOUND('',#523,.T.);
#125=FACE_BOUND('',#525,.T.);
#126=FACE_BOUND('',#531,.T.);
#127=FACE_BOUND('',#534,.T.);
#128=FACE_BOUND('',#536,.T.);
#129=FACE_BOUND('',#538,.T.);
#130=FACE_BOUND('',#544,.T.);
#131=FACE_BOUND('',#548,.T.);
#132=FACE_BOUND('',#550,.T.);
#133=FACE_BOUND('',#553,.T.);
#134=FACE_BOUND('',#568,.T.);
#135=B_SPLINE_CURVE_WITH_KNOTS('',3,(#7651,#7652,#7653,#7654,#7655,#7656,
#7657,#7658,#7659,#7660,#7661,#7662,#7663,#7664,#7665,#7666,#7667,#7668),
 .UNSPECIFIED.,.F.,.F.,(4,2,2,2,2,2,2,2,4),(3.01498157723135,3.39185457770905,
3.76872757818674,4.14559997201688,4.52247236584703,4.89934475967718,5.27621715350733,
5.65309015398502,6.02996315446271),.UNSPECIFIED.);
#136=B_SPLINE_CURVE_WITH_KNOTS('',3,(#7669,#7670,#7671,#7672,#7673,#7674,
#7675,#7676,#7677,#7678,#7679,#7680,#7681,#7682,#7683,#7684,#7685,#7686),
 .UNSPECIFIED.,.F.,.F.,(4,2,2,2,2,2,2,2,4),(6.02996315446271,6.4068361549404,
6.78370915541809,7.16058154924824,7.53745394307838,7.91432633690853,8.29119873073868,
8.66807173121637,9.04494473169406),.UNSPECIFIED.);
#137=B_SPLINE_CURVE_WITH_KNOTS('',3,(#7689,#7690,#7691,#7692,#7693,#7694,
#7695,#7696,#7697,#7698,#7699,#7700,#7701,#7702,#7703,#7704,#7705,#7706),
 .UNSPECIFIED.,.F.,.F.,(4,2,2,2,2,2,2,2,4),(0.,0.376873000477691,0.753746000955381,
1.13061839478553,1.50749078861568,1.88436318244582,2.26123557627597,2.63810857675366,
3.01498157723135),.UNSPECIFIED.);
#138=B_SPLINE_CURVE_WITH_KNOTS('',3,(#7707,#7708,#7709,#7710,#7711,#7712,
#7713,#7714,#7715,#7716,#7717,#7718,#7719,#7720,#7721,#7722,#7723,#7724),
 .UNSPECIFIED.,.F.,.F.,(4,2,2,2,2,2,2,2,4),(3.01498157723135,3.39185457770904,
3.76872757818674,4.14559997201688,4.52247236584703,4.89934475967718,5.27621715350733,
5.65309015398502,6.02996315446271),.UNSPECIFIED.);
#139=B_SPLINE_CURVE_WITH_KNOTS('',3,(#11078,#11079,#11080,#11081,#11082,
#11083,#11084,#11085,#11086,#11087,#11088,#11089,#11090,#11091,#11092,#11093,
#11094,#11095,#11096,#11097,#11098,#11099,#11100,#11101,#11102,#11103,#11104,
#11105,#11106,#11107),.UNSPECIFIED.,.F.,.F.,(4,2,2,2,2,2,2,2,2,2,2,2,2,
2,4),(-4.18591455437331,-3.91515878973024,-3.64440302508717,-3.3736472604441,
-3.10289149580103,-2.59792438649385,-2.34544083184025,-2.09295727718666,
-1.84047372253307,-1.58799016787947,-1.08302305857229,-0.812267293929217,
-0.541511529286145,-0.270755764643072,0.),.UNSPECIFIED.);
#140=B_SPLINE_CURVE_WITH_KNOTS('',3,(#11108,#11109,#11110,#11111,#11112,
#11113,#11114,#11115,#11116,#11117,#11118,#11119,#11120,#11121,#11122,#11123,
#11124,#11125,#11126,#11127,#11128,#11129,#11130,#11131,#11132,#11133,#11134,
#11135,#11136,#11137),.UNSPECIFIED.,.F.,.F.,(4,2,2,2,2,2,2,2,2,2,2,2,2,
2,4),(0.,0.270755764643072,0.541511529286144,0.812267293929215,1.08302305857229,
1.58799016787947,1.84047372253307,2.09295727718666,2.34544083184025,2.59792438649385,
3.10289149580103,3.3736472604441,3.64440302508717,3.91515878973024,4.18591455437331),
 .UNSPECIFIED.);
#141=B_SPLINE_CURVE_WITH_KNOTS('',3,(#11155,#11156,#11157,#11158,#11159,
#11160,#11161,#11162,#11163,#11164,#11165,#11166,#11167,#11168,#11169,#11170,
#11171,#11172,#11173,#11174,#11175,#11176,#11177,#11178,#11179,#11180,#11181,
#11182,#11183,#11184),.UNSPECIFIED.,.F.,.F.,(4,2,2,2,2,2,2,2,2,2,2,2,2,
2,4),(4.53865697324691,4.83291964941679,5.12718232558667,5.42144500175655,
5.71570767792644,6.2618465688984,6.53491601438438,6.80798545987036,7.08105490535634,
7.35412435084232,7.90026324181428,8.19452591798416,8.48878859415405,8.78305127032393,
9.07731394649381),.UNSPECIFIED.);
#142=B_SPLINE_CURVE_WITH_KNOTS('',3,(#11185,#11186,#11187,#11188,#11189,
#11190,#11191,#11192,#11193,#11194,#11195,#11196,#11197,#11198,#11199,#11200,
#11201,#11202,#11203,#11204,#11205,#11206,#11207,#11208,#11209,#11210,#11211,
#11212,#11213,#11214),.UNSPECIFIED.,.F.,.F.,(4,2,2,2,2,2,2,2,2,2,2,2,2,
2,4),(9.07731394649381,9.3715766226637,9.66583929883358,9.96010197500346,
10.2543646511733,10.8005035421453,11.0735729876313,11.3466424331173,11.6197118786033,
11.8927813240892,12.4389202150612,12.7331828912311,13.027445567401,13.3217082435708,
13.6159709197407),.UNSPECIFIED.);
#143=B_SPLINE_CURVE_WITH_KNOTS('',3,(#11375,#11376,#11377,#11378),
 .UNSPECIFIED.,.F.,.F.,(4,4),(-1.,-0.998645968698766),.UNSPECIFIED.);
#144=B_SPLINE_CURVE_WITH_KNOTS('',3,(#11385,#11386,#11387,#11388,#11389,
#11390,#11391,#11392,#11393,#11394,#11395,#11396,#11397,#11398,#11399,#11400,
#11401,#11402,#11403,#11404,#11405,#11406,#11407,#11408,#11409,#11410,#11411,
#11412,#11413,#11414,#11415,#11416,#11417,#11418,#11419,#11420,#11421,#11422,
#11423,#11424,#11425,#11426,#11427,#11428,#11429,#11430,#11431,#11432,#11433,
#11434,#11435,#11436,#11437,#11438,#11439,#11440,#11441,#11442,#11443,#11444,
#11445,#11446,#11447,#11448,#11449,#11450,#11451,#11452,#11453,#11454,#11455,
#11456,#11457,#11458,#11459,#11460,#11461,#11462,#11463,#11464,#11465,#11466,
#11467,#11468,#11469,#11470,#11471,#11472,#11473,#11474,#11475,#11476,#11477,
#11478,#11479,#11480,#11481,#11482,#11483,#11484,#11485,#11486,#11487,#11488,
#11489,#11490,#11491,#11492,#11493,#11494,#11495,#11496,#11497,#11498,#11499,
#11500,#11501,#11502,#11503,#11504,#11505,#11506,#11507,#11508,#11509,#11510,
#11511,#11512,#11513,#11514,#11515,#11516,#11517,#11518,#11519,#11520,#11521,
#11522,#11523,#11524,#11525,#11526,#11527,#11528,#11529,#11530,#11531,#11532,
#11533,#11534,#11535,#11536,#11537,#11538,#11539,#11540,#11541,#11542,#11543,
#11544,#11545,#11546,#11547,#11548,#11549,#11550,#11551,#11552,#11553,#11554,
#11555,#11556,#11557,#11558,#11559,#11560,#11561,#11562,#11563,#11564,#11565,
#11566,#11567,#11568,#11569,#11570,#11571,#11572,#11573,#11574,#11575,#11576,
#11577,#11578,#11579,#11580,#11581,#11582,#11583,#11584,#11585,#11586,#11587,
#11588,#11589,#11590,#11591,#11592,#11593,#11594,#11595,#11596,#11597,#11598,
#11599,#11600,#11601,#11602,#11603,#11604,#11605,#11606,#11607,#11608,#11609,
#11610,#11611,#11612,#11613,#11614,#11615,#11616,#11617,#11618,#11619,#11620,
#11621,#11622,#11623,#11624,#11625,#11626,#11627,#11628,#11629,#11630,#11631,
#11632,#11633,#11634,#11635,#11636,#11637,#11638,#11639,#11640,#11641,#11642,
#11643,#11644,#11645,#11646,#11647,#11648,#11649,#11650,#11651,#11652,#11653,
#11654,#11655,#11656,#11657,#11658,#11659,#11660,#11661,#11662,#11663,#11664,
#11665,#11666,#11667,#11668,#11669,#11670,#11671,#11672,#11673,#11674,#11675,
#11676,#11677,#11678,#11679,#11680,#11681,#11682,#11683,#11684,#11685,#11686,
#11687,#11688,#11689,#11690,#11691,#11692,#11693,#11694,#11695,#11696,#11697,
#11698,#11699,#11700,#11701,#11702,#11703,#11704,#11705,#11706,#11707,#11708,
#11709,#11710,#11711,#11712,#11713,#11714,#11715,#11716,#11717,#11718,#11719,
#11720,#11721,#11722,#11723,#11724,#11725,#11726,#11727,#11728,#11729,#11730,
#11731,#11732,#11733,#11734,#11735,#11736,#11737,#11738,#11739,#11740,#11741,
#11742),.UNSPECIFIED.,.F.,.F.,(4,3,3,3,3,3,3,3,3,3,3,3,3,3,3,3,3,3,3,3,
3,3,3,3,3,3,3,3,3,3,3,3,3,3,3,3,3,3,3,3,3,3,3,3,3,3,3,3,3,3,3,3,3,3,3,3,
3,3,3,3,3,3,3,3,3,3,3,3,3,3,3,3,3,3,3,3,3,3,3,3,3,3,3,3,3,3,3,3,3,3,3,3,
3,3,3,3,3,3,3,3,3,3,3,3,3,3,3,3,3,3,3,3,3,3,3,3,3,3,3,4),(-0.331979302032099,
-0.328745544947817,-0.325511126349503,-0.322277581756429,-0.319042795051795,
-0.316666666666667,-0.313432410645245,-0.310074307983934,-0.306840488099785,
-0.303607230746873,-0.300373105768056,-0.3,-0.296765743978578,-0.293407641317267,
-0.290173821433118,-0.286940564080179,-0.283706439101408,-0.283333333333333,
-0.280099077311897,-0.27674097465059,-0.273507154766441,-0.270273897413541,
-0.267039772434759,-0.266666666666667,-0.263432410645244,-0.260074307983933,
-0.25684048809978,-0.253607230746841,-0.250373105768036,-0.25,-0.246765743978575,
-0.243407641317264,-0.240173821433105,-0.236940564080198,-0.233706439101398,
-0.233333333333333,-0.230099077311924,-0.22674097465061,-0.223507154766454,
-0.220273897413536,-0.217039772434708,-0.216666666666667,-0.213432410645268,
-0.210074307983951,-0.206840488099798,-0.203607230746877,-0.200373105768084,
-0.2,-0.196765743978578,-0.193407641317267,-0.190173821433123,-0.186940564080229,
-0.183706439101414,-0.183333333333333,-0.180099077311908,-0.176740974650597,
-0.173507154766428,-0.170273897413483,-0.167039772434678,-0.166666666666667,
-0.163432410645259,-0.160074307983944,-0.156840488099797,-0.153607230746853,
-0.150373105768069,-0.15,-0.146765743978574,-0.143407641317264,-0.140173821433101,
-0.136940564080169,-0.133706439101386,-0.133333333333333,-0.130099077311911,
-0.1267409746506,-0.123507154766447,-0.120273897413526,-0.117039772434722,
-0.116666666666667,-0.113432410645241,-0.110074307983931,-0.106840488099774,
-0.103607230746858,-0.10037310576804,-0.1,-0.0967657439785776,-0.0934076413172665,
-0.0901738214331063,-0.0869405640801917,-0.0837064391013879,-0.0833333333333334,
-0.0800990773119075,-0.0767409746505973,-0.0735071547664396,-0.0702738974135466,
-0.0670397724347522,-0.0666666666666667,-0.0634324106452447,-0.0600743079839336,
-0.0568404880997839,-0.0536072307468639,-0.0503731057680767,-0.05,-0.0467657439785748,
-0.0434076413172644,-0.0401738214331216,-0.0369405640801967,-0.033706439101418,
-0.0333333333333333,-0.030099077311911,-0.0267409746505999,-0.0235071547664523,
-0.0202738974135343,-0.017039772434738,-0.0166666666666667,-0.0134324106517174,
-0.0100743318149406,-0.00684051195133032,-0.00360725461687006,-0.000373129688631168,
-9.53046099950368E-8),.UNSPECIFIED.);
#145=B_SPLINE_CURVE_WITH_KNOTS('',3,(#11789,#11790,#11791,#11792,#11793,
#11794,#11795,#11796,#11797,#11798,#11799,#11800,#11801,#11802,#11803,#11804,
#11805,#11806,#11807,#11808,#11809,#11810,#11811,#11812,#11813,#11814,#11815,
#11816,#11817,#11818,#11819,#11820,#11821,#11822,#11823,#11824,#11825,#11826,
#11827,#11828,#11829,#11830,#11831,#11832,#11833,#11834,#11835,#11836,#11837,
#11838,#11839,#11840,#11841,#11842,#11843,#11844,#11845,#11846,#11847,#11848,
#11849,#11850,#11851,#11852,#11853,#11854,#11855,#11856,#11857,#11858,#11859,
#11860,#11861,#11862,#11863,#11864,#11865,#11866,#11867,#11868,#11869,#11870,
#11871,#11872,#11873,#11874,#11875,#11876,#11877,#11878,#11879,#11880,#11881,
#11882,#11883,#11884,#11885,#11886,#11887,#11888,#11889,#11890,#11891,#11892,
#11893,#11894,#11895,#11896,#11897,#11898,#11899,#11900,#11901,#11902,#11903,
#11904,#11905,#11906,#11907,#11908,#11909,#11910,#11911,#11912,#11913,#11914,
#11915,#11916,#11917,#11918,#11919,#11920,#11921,#11922,#11923,#11924,#11925,
#11926,#11927,#11928,#11929,#11930,#11931,#11932,#11933,#11934,#11935,#11936,
#11937,#11938,#11939,#11940,#11941,#11942,#11943,#11944,#11945,#11946,#11947,
#11948,#11949,#11950,#11951,#11952,#11953,#11954,#11955,#11956,#11957,#11958,
#11959,#11960,#11961,#11962,#11963,#11964,#11965,#11966,#11967,#11968,#11969,
#11970,#11971,#11972,#11973,#11974,#11975,#11976,#11977,#11978,#11979,#11980,
#11981,#11982,#11983,#11984,#11985,#11986,#11987,#11988,#11989,#11990,#11991,
#11992,#11993,#11994,#11995,#11996,#11997,#11998,#11999,#12000,#12001,#12002,
#12003,#12004,#12005,#12006,#12007,#12008,#12009,#12010,#12011,#12012,#12013,
#12014,#12015,#12016,#12017,#12018,#12019,#12020,#12021,#12022,#12023,#12024,
#12025,#12026,#12027,#12028,#12029,#12030,#12031,#12032,#12033,#12034,#12035,
#12036,#12037,#12038,#12039,#12040,#12041,#12042,#12043,#12044,#12045,#12046,
#12047,#12048,#12049,#12050,#12051,#12052,#12053,#12054,#12055,#12056,#12057,
#12058,#12059,#12060,#12061,#12062,#12063,#12064,#12065,#12066,#12067,#12068,
#12069,#12070,#12071,#12072,#12073,#12074,#12075,#12076,#12077,#12078,#12079,
#12080,#12081,#12082,#12083,#12084,#12085,#12086,#12087,#12088,#12089,#12090,
#12091,#12092,#12093,#12094,#12095,#12096,#12097,#12098,#12099,#12100,#12101,
#12102,#12103,#12104,#12105,#12106,#12107,#12108,#12109,#12110,#12111,#12112,
#12113,#12114,#12115,#12116,#12117,#12118,#12119,#12120,#12121,#12122,#12123,
#12124,#12125,#12126,#12127,#12128,#12129,#12130,#12131,#12132,#12133,#12134,
#12135,#12136,#12137,#12138,#12139,#12140,#12141,#12142,#12143,#12144,#12145,
#12146,#12147,#12148,#12149),.UNSPECIFIED.,.F.,.F.,(4,3,3,3,3,3,3,3,3,3,
3,3,3,3,3,3,3,3,3,3,3,3,3,3,3,3,3,3,3,3,3,3,3,3,3,3,3,3,3,3,3,3,3,3,3,3,
3,3,3,3,3,3,3,3,3,3,3,3,3,3,3,3,3,3,3,3,3,3,3,3,3,3,3,3,3,3,3,3,3,3,3,3,
3,3,3,3,3,3,3,3,3,3,3,3,3,3,3,3,3,3,3,3,3,3,3,3,3,3,3,3,3,3,3,3,3,3,3,3,
3,3,4),(-0.665312635365433,-0.662078878281142,-0.658844459682826,-0.655610915089758,
-0.652376128385123,-0.65,-0.646765743978579,-0.643407641317267,-0.640173821433118,
-0.636940564080195,-0.633706439101402,-0.633333333333333,-0.630099077311912,
-0.626740974650601,-0.623507154766448,-0.620273897413523,-0.617039772434729,
-0.616666666666667,-0.613432410645243,-0.610074307983932,-0.60684048809978,
-0.603607230746855,-0.60037310576806,-0.6,-0.596765743978578,-0.593407641317267,
-0.590173821433114,-0.586940564080189,-0.583706439101395,-0.583333333333333,
-0.580099077311911,-0.5767409746506,-0.573507154766447,-0.570273897413521,
-0.567039772434727,-0.566666666666667,-0.563432410645245,-0.560074307983934,
-0.556840488099781,-0.553607230746856,-0.550373105768065,-0.55,-0.546765743978579,
-0.543407641317267,-0.540173821433115,-0.536940564080189,-0.533706439101384,
-0.533333333333333,-0.530099077311911,-0.5267409746506,-0.523507154766446,
-0.52027389741352,-0.517039772434727,-0.516666666666667,-0.513432410645245,
-0.510074307983934,-0.506840488099781,-0.503607230746855,-0.500373105768063,
-0.5,-0.496765743978578,-0.493407641317267,-0.490173821433103,-0.486940564080178,
-0.483706439101384,-0.483333333333333,-0.480099077311911,-0.4767409746506,
-0.473507154766447,-0.47027389741351,-0.467039772434717,-0.466666666666667,
-0.463432410645245,-0.460074307983933,-0.456840488099777,-0.453607230746852,
-0.450373105768059,-0.45,-0.446765743978577,-0.443407641317266,-0.440173821433109,
-0.43694056408017,-0.433706439101377,-0.433333333333333,-0.430099077311911,
-0.4267409746506,-0.423507154766447,-0.420273897413509,-0.417039772434716,
-0.416666666666667,-0.413432410645244,-0.410074307983933,-0.40684048809978,
-0.403607230746867,-0.400373105768075,-0.4,-0.396765743978578,-0.393407641317267,
-0.390173821433118,-0.386940564080206,-0.383706439101414,-0.383333333333333,
-0.380099077311912,-0.376740974650601,-0.373507154766456,-0.370273897413568,
-0.367039772434754,-0.366666666666667,-0.363432410645244,-0.360074307983933,
-0.356840488099784,-0.353607230746845,-0.350373105768042,-0.35,-0.346765743978578,
-0.343407641317267,-0.34017382143311,-0.336940564080171,-0.333706439101378,
-0.333333333333333,-0.331979302032099),.UNSPECIFIED.);
#146=B_SPLINE_CURVE_WITH_KNOTS('',3,(#12194,#12195,#12196,#12197,#12198,
#12199,#12200,#12201,#12202,#12203,#12204,#12205,#12206,#12207,#12208,#12209,
#12210,#12211,#12212,#12213,#12214,#12215,#12216,#12217,#12218,#12219,#12220,
#12221,#12222,#12223,#12224,#12225,#12226,#12227,#12228,#12229,#12230,#12231,
#12232,#12233,#12234,#12235,#12236,#12237,#12238,#12239,#12240,#12241,#12242,
#12243,#12244,#12245,#12246,#12247,#12248,#12249,#12250,#12251,#12252,#12253,
#12254,#12255,#12256,#12257,#12258,#12259,#12260,#12261,#12262,#12263,#12264,
#12265,#12266,#12267,#12268,#12269,#12270,#12271,#12272,#12273,#12274,#12275,
#12276,#12277,#12278,#12279,#12280,#12281,#12282,#12283,#12284,#12285,#12286,
#12287,#12288,#12289,#12290,#12291,#12292,#12293,#12294,#12295,#12296,#12297,
#12298,#12299,#12300,#12301,#12302,#12303,#12304,#12305,#12306,#12307,#12308,
#12309,#12310,#12311,#12312,#12313,#12314,#12315,#12316,#12317,#12318,#12319,
#12320,#12321,#12322,#12323,#12324,#12325,#12326,#12327,#12328,#12329,#12330,
#12331,#12332,#12333,#12334,#12335,#12336,#12337,#12338,#12339,#12340,#12341,
#12342,#12343,#12344,#12345,#12346,#12347,#12348,#12349,#12350,#12351,#12352,
#12353,#12354,#12355,#12356,#12357,#12358,#12359,#12360,#12361,#12362,#12363,
#12364,#12365,#12366,#12367,#12368,#12369,#12370,#12371,#12372,#12373,#12374,
#12375,#12376,#12377,#12378,#12379,#12380,#12381,#12382,#12383,#12384,#12385,
#12386,#12387,#12388,#12389,#12390,#12391,#12392,#12393,#12394,#12395,#12396,
#12397,#12398,#12399,#12400,#12401,#12402,#12403,#12404,#12405,#12406,#12407,
#12408,#12409,#12410,#12411,#12412,#12413,#12414,#12415,#12416,#12417,#12418,
#12419,#12420,#12421,#12422,#12423,#12424,#12425,#12426,#12427,#12428,#12429,
#12430,#12431,#12432,#12433,#12434,#12435,#12436,#12437,#12438,#12439,#12440,
#12441,#12442,#12443,#12444,#12445,#12446,#12447,#12448,#12449,#12450,#12451,
#12452,#12453,#12454,#12455,#12456,#12457,#12458,#12459,#12460,#12461,#12462,
#12463,#12464,#12465,#12466,#12467,#12468,#12469,#12470,#12471,#12472,#12473,
#12474,#12475,#12476,#12477,#12478,#12479,#12480,#12481,#12482,#12483,#12484,
#12485,#12486,#12487,#12488,#12489,#12490,#12491,#12492,#12493,#12494,#12495,
#12496,#12497,#12498,#12499,#12500,#12501,#12502,#12503,#12504,#12505,#12506,
#12507,#12508,#12509,#12510,#12511,#12512,#12513,#12514,#12515,#12516,#12517,
#12518,#12519,#12520,#12521,#12522,#12523,#12524,#12525,#12526,#12527,#12528,
#12529,#12530,#12531,#12532,#12533,#12534,#12535,#12536,#12537,#12538,#12539,
#12540,#12541,#12542,#12543,#12544,#12545,#12546,#12547,#12548,#12549,#12550,
#12551,#12552,#12553,#12554),.UNSPECIFIED.,.F.,.F.,(4,3,3,3,3,3,3,3,3,3,
3,3,3,3,3,3,3,3,3,3,3,3,3,3,3,3,3,3,3,3,3,3,3,3,3,3,3,3,3,3,3,3,3,3,3,3,
3,3,3,3,3,3,3,3,3,3,3,3,3,3,3,3,3,3,3,3,3,3,3,3,3,3,3,3,3,3,3,3,3,3,3,3,
3,3,3,3,3,3,3,3,3,3,3,3,3,3,3,3,3,3,3,3,3,3,3,3,3,3,3,3,3,3,3,3,3,3,3,3,
3,3,4),(-0.998645968698766,-0.995412211614476,-0.99217779301616,-0.988944248423087,
-0.985709461718452,-0.983333333333333,-0.980099077311911,-0.9767409746506,
-0.973507154766447,-0.970273897413519,-0.967039772434726,-0.966666666666667,
-0.963432410645243,-0.960074307983932,-0.956840488099779,-0.953607230746854,
-0.950373105768062,-0.95,-0.946765743978577,-0.943407641317266,-0.940173821433113,
-0.936940564080185,-0.933706439101392,-0.933333333333333,-0.930099077311911,
-0.9267409746506,-0.923507154766446,-0.92027389741352,-0.917039772434728,
-0.916666666666667,-0.913432410645244,-0.910074307983933,-0.90684048809978,
-0.903607230746854,-0.90037310576806,-0.9,-0.896765743978578,-0.893407641317267,
-0.890173821433115,-0.886940564080189,-0.883706439101396,-0.883333333333333,
-0.880099077311911,-0.8767409746506,-0.873507154766449,-0.870273897413525,
-0.867039772434733,-0.866666666666667,-0.863432410645245,-0.860074307983934,
-0.856840488099781,-0.853607230746854,-0.850373105768058,-0.85,-0.846765743978578,
-0.843407641317267,-0.840173821433114,-0.836940564080188,-0.833706439101395,
-0.833333333333333,-0.830099077311911,-0.8267409746506,-0.823507154766447,
-0.820273897413526,-0.817039772434731,-0.816666666666667,-0.81343241064524,
-0.81007430798393,-0.806840488099777,-0.803607230746853,-0.800373105768059,
-0.8,-0.796765743978579,-0.793407641317267,-0.790173821433115,-0.786940564080183,
-0.783706439101388,-0.783333333333333,-0.780099077311911,-0.7767409746506,
-0.773507154766446,-0.770273897413509,-0.767039772434712,-0.766666666666667,
-0.763432410645249,-0.760074307983936,-0.756840488099782,-0.753607230746868,
-0.75037310576807,-0.75,-0.746765743978578,-0.743407641317267,-0.740173821433118,
-0.736940564080168,-0.733706439101356,-0.733333333333333,-0.730099077311911,
-0.7267409746506,-0.723507154766451,-0.720273897413524,-0.717039772434739,
-0.716666666666667,-0.713432410645237,-0.710074307983928,-0.706840488099775,
-0.703607230746849,-0.700373105768067,-0.7,-0.69676574397857,-0.693407641317261,
-0.690173821433107,-0.686940564080183,-0.683706439101389,-0.683333333333333,
-0.680099077311912,-0.6767409746506,-0.673507154766448,-0.670273897413522,
-0.667039772434727,-0.666666666666667,-0.665312635365433),.UNSPECIFIED.);
#147=B_SPLINE_CURVE_WITH_KNOTS('',3,(#12558,#12559,#12560,#12561,#12562,
#12563),.UNSPECIFIED.,.F.,.F.,(4,2,4),(-4.25163970020424,-2.12588055073164,
0.),.UNSPECIFIED.);
#148=B_SPLINE_CURVE_WITH_KNOTS('',3,(#12569,#12570,#12571,#12572,#12573,
#12574),.UNSPECIFIED.,.F.,.F.,(4,2,4),(-4.25163970020424,-2.1257591494726,
0.),.UNSPECIFIED.);
#149=CIRCLE('',#3091,105.5);
#150=CIRCLE('',#3140,105.5);
#151=CIRCLE('',#3142,120.5);
#152=CIRCLE('',#3143,120.5);
#153=CIRCLE('',#3144,120.5);
#154=CIRCLE('',#3147,118.168461709225);
#155=CIRCLE('',#3148,115.5);
#156=CIRCLE('',#3150,114.726497308104);
#157=CIRCLE('',#3151,105.5);
#158=CIRCLE('',#3153,114.797295826488);
#159=CIRCLE('',#3160,10.);
#160=CIRCLE('',#3163,10.);
#161=CIRCLE('',#3169,12.);
#162=CIRCLE('',#3171,15.);
#163=CIRCLE('',#3172,15.);
#164=CIRCLE('',#3174,9.99999999999999);
#165=CIRCLE('',#3176,9.99999999999998);
#166=CIRCLE('',#3184,12.5);
#167=CIRCLE('',#3186,15.);
#168=CIRCLE('',#3187,14.);
#169=CIRCLE('',#3189,15.);
#170=CIRCLE('',#3190,14.);
#171=CIRCLE('',#3194,13.5);
#172=CIRCLE('',#3196,12.5);
#173=CIRCLE('',#3198,12.5);
#174=CIRCLE('',#3200,11.5);
#175=CIRCLE('',#3202,11.5);
#176=CIRCLE('',#3206,202.);
#177=CIRCLE('',#3207,200.);
#178=CIRCLE('',#3209,52.);
#179=CIRCLE('',#3211,50.);
#180=CIRCLE('',#3213,50.);
#181=CIRCLE('',#3215,52.);
#182=CIRCLE('',#3216,52.);
#183=CIRCLE('',#3219,56.);
#184=CIRCLE('',#3220,56.);
#185=CIRCLE('',#3225,15.);
#186=CIRCLE('',#3226,14.);
#187=CIRCLE('',#3228,15.);
#188=CIRCLE('',#3229,15.);
#189=CIRCLE('',#3230,65.0000000000001);
#190=CIRCLE('',#3232,15.);
#191=CIRCLE('',#3234,66.0000000000001);
#192=CIRCLE('',#3235,14.);
#193=CIRCLE('',#3236,14.);
#194=CIRCLE('',#3238,14.);
#195=CIRCLE('',#3240,11.);
#196=CIRCLE('',#3242,12.5);
#197=CIRCLE('',#3243,12.5);
#198=CIRCLE('',#3245,11.5);
#199=CIRCLE('',#3246,11.5);
#200=CIRCLE('',#3249,11.);
#201=CIRCLE('',#3254,7.5);
#202=CIRCLE('',#3255,1859.05088195134);
#203=CIRCLE('',#3257,7.5);
#204=CIRCLE('',#3258,1859.05088195135);
#205=CIRCLE('',#3264,25.);
#206=CIRCLE('',#3265,25.);
#207=FACE_OUTER_BOUND('',#377,.T.);
#208=FACE_OUTER_BOUND('',#378,.T.);
#209=FACE_OUTER_BOUND('',#379,.T.);
#210=FACE_OUTER_BOUND('',#380,.T.);
#211=FACE_OUTER_BOUND('',#381,.T.);
#212=FACE_OUTER_BOUND('',#382,.T.);
#213=FACE_OUTER_BOUND('',#383,.T.);
#214=FACE_OUTER_BOUND('',#384,.T.);
#215=FACE_OUTER_BOUND('',#385,.T.);
#216=FACE_OUTER_BOUND('',#386,.T.);
#217=FACE_OUTER_BOUND('',#387,.T.);
#218=FACE_OUTER_BOUND('',#388,.T.);
#219=FACE_OUTER_BOUND('',#389,.T.);
#220=FACE_OUTER_BOUND('',#390,.T.);
#221=FACE_OUTER_BOUND('',#391,.T.);
#222=FACE_OUTER_BOUND('',#392,.T.);
#223=FACE_OUTER_BOUND('',#393,.T.);
#224=FACE_OUTER_BOUND('',#394,.T.);
#225=FACE_OUTER_BOUND('',#395,.T.);
#226=FACE_OUTER_BOUND('',#396,.T.);
#227=FACE_OUTER_BOUND('',#397,.T.);
#228=FACE_OUTER_BOUND('',#398,.T.);
#229=FACE_OUTER_BOUND('',#399,.T.);
#230=FACE_OUTER_BOUND('',#400,.T.);
#231=FACE_OUTER_BOUND('',#401,.T.);
#232=FACE_OUTER_BOUND('',#402,.T.);
#233=FACE_OUTER_BOUND('',#403,.T.);
#234=FACE_OUTER_BOUND('',#404,.T.);
#235=FACE_OUTER_BOUND('',#405,.T.);
#236=FACE_OUTER_BOUND('',#406,.T.);
#237=FACE_OUTER_BOUND('',#407,.T.);
#238=FACE_OUTER_BOUND('',#408,.T.);
#239=FACE_OUTER_BOUND('',#409,.T.);
#240=FACE_OUTER_BOUND('',#410,.T.);
#241=FACE_OUTER_BOUND('',#411,.T.);
#242=FACE_OUTER_BOUND('',#412,.T.);
#243=FACE_OUTER_BOUND('',#413,.T.);
#244=FACE_OUTER_BOUND('',#414,.T.);
#245=FACE_OUTER_BOUND('',#415,.T.);
#246=FACE_OUTER_BOUND('',#416,.T.);
#247=FACE_OUTER_BOUND('',#417,.T.);
#248=FACE_OUTER_BOUND('',#418,.T.);
#249=FACE_OUTER_BOUND('',#419,.T.);
#250=FACE_OUTER_BOUND('',#420,.T.);
#251=FACE_OUTER_BOUND('',#421,.T.);
#252=FACE_OUTER_BOUND('',#422,.T.);
#253=FACE_OUTER_BOUND('',#423,.T.);
#254=FACE_OUTER_BOUND('',#424,.T.);
#255=FACE_OUTER_BOUND('',#425,.T.);
#256=FACE_OUTER_BOUND('',#426,.T.);
#257=FACE_OUTER_BOUND('',#427,.T.);
#258=FACE_OUTER_BOUND('',#428,.T.);
#259=FACE_OUTER_BOUND('',#429,.T.);
#260=FACE_OUTER_BOUND('',#430,.T.);
#261=FACE_OUTER_BOUND('',#431,.T.);
#262=FACE_OUTER_BOUND('',#432,.T.);
#263=FACE_OUTER_BOUND('',#433,.T.);
#264=FACE_OUTER_BOUND('',#434,.T.);
#265=FACE_OUTER_BOUND('',#435,.T.);
#266=FACE_OUTER_BOUND('',#436,.T.);
#267=FACE_OUTER_BOUND('',#437,.T.);
#268=FACE_OUTER_BOUND('',#438,.T.);
#269=FACE_OUTER_BOUND('',#439,.T.);
#270=FACE_OUTER_BOUND('',#440,.T.);
#271=FACE_OUTER_BOUND('',#441,.T.);
#272=FACE_OUTER_BOUND('',#442,.T.);
#273=FACE_OUTER_BOUND('',#443,.T.);
#274=FACE_OUTER_BOUND('',#444,.T.);
#275=FACE_OUTER_BOUND('',#445,.T.);
#276=FACE_OUTER_BOUND('',#446,.T.);
#277=FACE_OUTER_BOUND('',#447,.T.);
#278=FACE_OUTER_BOUND('',#448,.T.);
#279=FACE_OUTER_BOUND('',#449,.T.);
#280=FACE_OUTER_BOUND('',#450,.T.);
#281=FACE_OUTER_BOUND('',#451,.T.);
#282=FACE_OUTER_BOUND('',#452,.T.);
#283=FACE_OUTER_BOUND('',#453,.T.);
#284=FACE_OUTER_BOUND('',#454,.T.);
#285=FACE_OUTER_BOUND('',#455,.T.);
#286=FACE_OUTER_BOUND('',#456,.T.);
#287=FACE_OUTER_BOUND('',#457,.T.);
#288=FACE_OUTER_BOUND('',#458,.T.);
#289=FACE_OUTER_BOUND('',#459,.T.);
#290=FACE_OUTER_BOUND('',#460,.T.);
#291=FACE_OUTER_BOUND('',#461,.T.);
#292=FACE_OUTER_BOUND('',#462,.T.);
#293=FACE_OUTER_BOUND('',#463,.T.);
#294=FACE_OUTER_BOUND('',#464,.T.);
#295=FACE_OUTER_BOUND('',#465,.T.);
#296=FACE_OUTER_BOUND('',#466,.T.);
#297=FACE_OUTER_BOUND('',#467,.T.);
#298=FACE_OUTER_BOUND('',#468,.T.);
#299=FACE_OUTER_BOUND('',#469,.T.);
#300=FACE_OUTER_BOUND('',#470,.T.);
#301=FACE_OUTER_BOUND('',#471,.T.);
#302=FACE_OUTER_BOUND('',#472,.T.);
#303=FACE_OUTER_BOUND('',#473,.T.);
#304=FACE_OUTER_BOUND('',#474,.T.);
#305=FACE_OUTER_BOUND('',#475,.T.);
#306=FACE_OUTER_BOUND('',#476,.T.);
#307=FACE_OUTER_BOUND('',#479,.T.);
#308=FACE_OUTER_BOUND('',#480,.T.);
#309=FACE_OUTER_BOUND('',#482,.T.);
#310=FACE_OUTER_BOUND('',#484,.T.);
#311=FACE_OUTER_BOUND('',#486,.T.);
#312=FACE_OUTER_BOUND('',#487,.T.);
#313=FACE_OUTER_BOUND('',#488,.T.);
#314=FACE_OUTER_BOUND('',#489,.T.);
#315=FACE_OUTER_BOUND('',#490,.T.);
#316=FACE_OUTER_BOUND('',#491,.T.);
#317=FACE_OUTER_BOUND('',#492,.T.);
#318=FACE_OUTER_BOUND('',#493,.T.);
#319=FACE_OUTER_BOUND('',#494,.T.);
#320=FACE_OUTER_BOUND('',#495,.T.);
#321=FACE_OUTER_BOUND('',#496,.T.);
#322=FACE_OUTER_BOUND('',#497,.T.);
#323=FACE_OUTER_BOUND('',#498,.T.);
#324=FACE_OUTER_BOUND('',#499,.T.);
#325=FACE_OUTER_BOUND('',#500,.T.);
#326=FACE_OUTER_BOUND('',#501,.T.);
#327=FACE_OUTER_BOUND('',#503,.T.);
#328=FACE_OUTER_BOUND('',#504,.T.);
#329=FACE_OUTER_BOUND('',#505,.T.);
#330=FACE_OUTER_BOUND('',#506,.T.);
#331=FACE_OUTER_BOUND('',#507,.T.);
#332=FACE_OUTER_BOUND('',#509,.T.);
#333=FACE_OUTER_BOUND('',#511,.T.);
#334=FACE_OUTER_BOUND('',#513,.T.);
#335=FACE_OUTER_BOUND('',#515,.T.);
#336=FACE_OUTER_BOUND('',#516,.T.);
#337=FACE_OUTER_BOUND('',#518,.T.);
#338=FACE_OUTER_BOUND('',#519,.T.);
#339=FACE_OUTER_BOUND('',#521,.T.);
#340=FACE_OUTER_BOUND('',#522,.T.);
#341=FACE_OUTER_BOUND('',#524,.T.);
#342=FACE_OUTER_BOUND('',#526,.T.);
#343=FACE_OUTER_BOUND('',#527,.T.);
#344=FACE_OUTER_BOUND('',#528,.T.);
#345=FACE_OUTER_BOUND('',#529,.T.);
#346=FACE_OUTER_BOUND('',#530,.T.);
#347=FACE_OUTER_BOUND('',#532,.T.);
#348=FACE_OUTER_BOUND('',#533,.T.);
#349=FACE_OUTER_BOUND('',#535,.T.);
#350=FACE_OUTER_BOUND('',#537,.T.);
#351=FACE_OUTER_BOUND('',#539,.T.);
#352=FACE_OUTER_BOUND('',#540,.T.);
#353=FACE_OUTER_BOUND('',#541,.T.);
#354=FACE_OUTER_BOUND('',#542,.T.);
#355=FACE_OUTER_BOUND('',#543,.T.);
#356=FACE_OUTER_BOUND('',#545,.T.);
#357=FACE_OUTER_BOUND('',#546,.T.);
#358=FACE_OUTER_BOUND('',#547,.T.);
#359=FACE_OUTER_BOUND('',#549,.T.);
#360=FACE_OUTER_BOUND('',#551,.T.);
#361=FACE_OUTER_BOUND('',#552,.T.);
#362=FACE_OUTER_BOUND('',#554,.T.);
#363=FACE_OUTER_BOUND('',#555,.T.);
#364=FACE_OUTER_BOUND('',#556,.T.);
#365=FACE_OUTER_BOUND('',#557,.T.);
#366=FACE_OUTER_BOUND('',#558,.T.);
#367=FACE_OUTER_BOUND('',#559,.T.);
#368=FACE_OUTER_BOUND('',#560,.T.);
#369=FACE_OUTER_BOUND('',#561,.T.);
#370=FACE_OUTER_BOUND('',#562,.T.);
#371=FACE_OUTER_BOUND('',#563,.T.);
#372=FACE_OUTER_BOUND('',#564,.T.);
#373=FACE_OUTER_BOUND('',#565,.T.);
#374=FACE_OUTER_BOUND('',#566,.T.);
#375=FACE_OUTER_BOUND('',#567,.T.);
#376=FACE_OUTER_BOUND('',#569,.T.);
#377=EDGE_LOOP('',(#1803,#1804,#1805,#1806));
#378=EDGE_LOOP('',(#1807,#1808,#1809,#1810));
#379=EDGE_LOOP('',(#1811,#1812,#1813,#1814));
#380=EDGE_LOOP('',(#1815,#1816,#1817,#1818));
#381=EDGE_LOOP('',(#1819,#1820,#1821,#1822));
#382=EDGE_LOOP('',(#1823,#1824,#1825,#1826));
#383=EDGE_LOOP('',(#1827,#1828,#1829,#1830));
#384=EDGE_LOOP('',(#1831,#1832,#1833,#1834));
#385=EDGE_LOOP('',(#1835,#1836,#1837,#1838));
#386=EDGE_LOOP('',(#1839,#1840,#1841,#1842));
#387=EDGE_LOOP('',(#1843,#1844,#1845,#1846));
#388=EDGE_LOOP('',(#1847,#1848,#1849,#1850));
#389=EDGE_LOOP('',(#1851,#1852,#1853,#1854));
#390=EDGE_LOOP('',(#1855,#1856,#1857,#1858));
#391=EDGE_LOOP('',(#1859,#1860,#1861,#1862));
#392=EDGE_LOOP('',(#1863,#1864,#1865,#1866));
#393=EDGE_LOOP('',(#1867,#1868,#1869,#1870));
#394=EDGE_LOOP('',(#1871,#1872,#1873,#1874));
#395=EDGE_LOOP('',(#1875,#1876,#1877,#1878));
#396=EDGE_LOOP('',(#1879,#1880,#1881,#1882));
#397=EDGE_LOOP('',(#1883,#1884,#1885,#1886));
#398=EDGE_LOOP('',(#1887,#1888,#1889,#1890));
#399=EDGE_LOOP('',(#1891,#1892,#1893,#1894));
#400=EDGE_LOOP('',(#1895,#1896,#1897,#1898));
#401=EDGE_LOOP('',(#1899,#1900,#1901,#1902));
#402=EDGE_LOOP('',(#1903,#1904,#1905,#1906));
#403=EDGE_LOOP('',(#1907,#1908,#1909,#1910));
#404=EDGE_LOOP('',(#1911,#1912,#1913,#1914));
#405=EDGE_LOOP('',(#1915,#1916,#1917,#1918));
#406=EDGE_LOOP('',(#1919,#1920,#1921,#1922));
#407=EDGE_LOOP('',(#1923,#1924,#1925,#1926));
#408=EDGE_LOOP('',(#1927,#1928,#1929,#1930));
#409=EDGE_LOOP('',(#1931,#1932,#1933,#1934));
#410=EDGE_LOOP('',(#1935,#1936,#1937,#1938));
#411=EDGE_LOOP('',(#1939,#1940,#1941,#1942));
#412=EDGE_LOOP('',(#1943,#1944,#1945,#1946));
#413=EDGE_LOOP('',(#1947,#1948,#1949,#1950));
#414=EDGE_LOOP('',(#1951,#1952,#1953,#1954));
#415=EDGE_LOOP('',(#1955,#1956,#1957,#1958));
#416=EDGE_LOOP('',(#1959,#1960,#1961,#1962));
#417=EDGE_LOOP('',(#1963,#1964,#1965,#1966));
#418=EDGE_LOOP('',(#1967,#1968,#1969,#1970));
#419=EDGE_LOOP('',(#1971,#1972,#1973,#1974));
#420=EDGE_LOOP('',(#1975,#1976,#1977,#1978));
#421=EDGE_LOOP('',(#1979,#1980,#1981,#1982));
#422=EDGE_LOOP('',(#1983,#1984,#1985,#1986));
#423=EDGE_LOOP('',(#1987,#1988,#1989,#1990));
#424=EDGE_LOOP('',(#1991,#1992,#1993,#1994));
#425=EDGE_LOOP('',(#1995,#1996,#1997,#1998));
#426=EDGE_LOOP('',(#1999,#2000,#2001,#2002));
#427=EDGE_LOOP('',(#2003,#2004,#2005,#2006));
#428=EDGE_LOOP('',(#2007,#2008,#2009,#2010));
#429=EDGE_LOOP('',(#2011,#2012,#2013,#2014));
#430=EDGE_LOOP('',(#2015,#2016,#2017,#2018));
#431=EDGE_LOOP('',(#2019,#2020,#2021,#2022));
#432=EDGE_LOOP('',(#2023,#2024,#2025,#2026));
#433=EDGE_LOOP('',(#2027,#2028,#2029,#2030));
#434=EDGE_LOOP('',(#2031,#2032,#2033,#2034));
#435=EDGE_LOOP('',(#2035,#2036,#2037,#2038));
#436=EDGE_LOOP('',(#2039,#2040,#2041,#2042));
#437=EDGE_LOOP('',(#2043,#2044,#2045,#2046));
#438=EDGE_LOOP('',(#2047,#2048,#2049,#2050));
#439=EDGE_LOOP('',(#2051,#2052,#2053,#2054));
#440=EDGE_LOOP('',(#2055,#2056,#2057,#2058));
#441=EDGE_LOOP('',(#2059,#2060,#2061,#2062));
#442=EDGE_LOOP('',(#2063,#2064,#2065,#2066));
#443=EDGE_LOOP('',(#2067,#2068,#2069,#2070));
#444=EDGE_LOOP('',(#2071,#2072,#2073,#2074));
#445=EDGE_LOOP('',(#2075,#2076,#2077,#2078));
#446=EDGE_LOOP('',(#2079,#2080,#2081,#2082));
#447=EDGE_LOOP('',(#2083,#2084,#2085,#2086));
#448=EDGE_LOOP('',(#2087,#2088,#2089,#2090));
#449=EDGE_LOOP('',(#2091,#2092,#2093,#2094));
#450=EDGE_LOOP('',(#2095,#2096,#2097,#2098));
#451=EDGE_LOOP('',(#2099,#2100,#2101,#2102));
#452=EDGE_LOOP('',(#2103,#2104,#2105,#2106));
#453=EDGE_LOOP('',(#2107,#2108,#2109,#2110));
#454=EDGE_LOOP('',(#2111,#2112,#2113,#2114));
#455=EDGE_LOOP('',(#2115,#2116,#2117,#2118));
#456=EDGE_LOOP('',(#2119,#2120,#2121,#2122));
#457=EDGE_LOOP('',(#2123,#2124,#2125,#2126));
#458=EDGE_LOOP('',(#2127,#2128,#2129,#2130));
#459=EDGE_LOOP('',(#2131,#2132,#2133,#2134));
#460=EDGE_LOOP('',(#2135,#2136,#2137,#2138));
#461=EDGE_LOOP('',(#2139,#2140,#2141,#2142));
#462=EDGE_LOOP('',(#2143,#2144,#2145,#2146));
#463=EDGE_LOOP('',(#2147,#2148,#2149,#2150));
#464=EDGE_LOOP('',(#2151,#2152,#2153,#2154));
#465=EDGE_LOOP('',(#2155,#2156,#2157,#2158));
#466=EDGE_LOOP('',(#2159,#2160,#2161,#2162));
#467=EDGE_LOOP('',(#2163,#2164,#2165,#2166));
#468=EDGE_LOOP('',(#2167,#2168,#2169,#2170));
#469=EDGE_LOOP('',(#2171,#2172,#2173,#2174));
#470=EDGE_LOOP('',(#2175,#2176,#2177,#2178));
#471=EDGE_LOOP('',(#2179,#2180,#2181,#2182));
#472=EDGE_LOOP('',(#2183,#2184,#2185,#2186));
#473=EDGE_LOOP('',(#2187,#2188,#2189,#2190));
#474=EDGE_LOOP('',(#2191,#2192,#2193,#2194));
#475=EDGE_LOOP('',(#2195,#2196,#2197,#2198,#2199,#2200,#2201,#2202));
#476=EDGE_LOOP('',(#2203,#2204,#2205,#2206,#2207));
#477=EDGE_LOOP('',(#2208,#2209));
#478=EDGE_LOOP('',(#2210,#2211));
#479=EDGE_LOOP('',(#2212,#2213,#2214,#2215));
#480=EDGE_LOOP('',(#2216));
#481=EDGE_LOOP('',(#2217));
#482=EDGE_LOOP('',(#2218));
#483=EDGE_LOOP('',(#2219,#2220));
#484=EDGE_LOOP('',(#2221));
#485=EDGE_LOOP('',(#2222));
#486=EDGE_LOOP('',(#2223,#2224,#2225,#2226));
#487=EDGE_LOOP('',(#2227,#2228,#2229,#2230));
#488=EDGE_LOOP('',(#2231,#2232,#2233,#2234));
#489=EDGE_LOOP('',(#2235,#2236,#2237,#2238,#2239,#2240,#2241,#2242,#2243,
#2244,#2245,#2246,#2247,#2248,#2249,#2250,#2251,#2252,#2253,#2254,#2255,
#2256,#2257,#2258,#2259,#2260,#2261,#2262,#2263,#2264,#2265,#2266,#2267,
#2268,#2269,#2270,#2271,#2272,#2273,#2274,#2275,#2276,#2277,#2278,#2279,
#2280,#2281,#2282,#2283,#2284,#2285,#2286,#2287,#2288,#2289,#2290,#2291,
#2292,#2293,#2294,#2295,#2296,#2297,#2298,#2299,#2300,#2301,#2302,#2303,
#2304,#2305,#2306,#2307,#2308,#2309,#2310,#2311,#2312,#2313,#2314,#2315,
#2316,#2317,#2318,#2319,#2320,#2321,#2322,#2323,#2324,#2325,#2326,#2327,
#2328,#2329,#2330,#2331,#2332,#2333,#2334,#2335,#2336,#2337,#2338));
#490=EDGE_LOOP('',(#2339,#2340,#2341,#2342));
#491=EDGE_LOOP('',(#2343,#2344,#2345,#2346,#2347,#2348,#2349,#2350,#2351,
#2352,#2353,#2354,#2355,#2356,#2357,#2358,#2359,#2360,#2361,#2362,#2363,
#2364,#2365,#2366,#2367,#2368,#2369,#2370,#2371,#2372,#2373,#2374,#2375,
#2376,#2377,#2378,#2379,#2380,#2381,#2382,#2383,#2384,#2385,#2386,#2387,
#2388,#2389,#2390,#2391,#2392,#2393,#2394,#2395,#2396,#2397,#2398,#2399,
#2400,#2401,#2402,#2403,#2404,#2405,#2406,#2407,#2408,#2409,#2410,#2411,
#2412,#2413,#2414,#2415,#2416,#2417,#2418,#2419,#2420,#2421,#2422,#2423,
#2424,#2425,#2426,#2427,#2428,#2429,#2430,#2431,#2432,#2433,#2434,#2435,
#2436,#2437,#2438,#2439,#2440,#2441,#2442,#2443,#2444,#2445,#2446));
#492=EDGE_LOOP('',(#2447,#2448,#2449));
#493=EDGE_LOOP('',(#2450,#2451,#2452,#2453,#2454));
#494=EDGE_LOOP('',(#2455));
#495=EDGE_LOOP('',(#2456,#2457,#2458,#2459,#2460));
#496=EDGE_LOOP('',(#2461));
#497=EDGE_LOOP('',(#2462,#2463,#2464,#2465));
#498=EDGE_LOOP('',(#2466,#2467,#2468,#2469,#2470));
#499=EDGE_LOOP('',(#2471));
#500=EDGE_LOOP('',(#2472,#2473,#2474,#2475));
#501=EDGE_LOOP('',(#2476));
#502=EDGE_LOOP('',(#2477));
#503=EDGE_LOOP('',(#2478,#2479,#2480,#2481));
#504=EDGE_LOOP('',(#2482));
#505=EDGE_LOOP('',(#2483,#2484,#2485,#2486));
#506=EDGE_LOOP('',(#2487,#2488,#2489,#2490,#2491));
#507=EDGE_LOOP('',(#2492));
#508=EDGE_LOOP('',(#2493));
#509=EDGE_LOOP('',(#2494));
#510=EDGE_LOOP('',(#2495));
#511=EDGE_LOOP('',(#2496,#2497,#2498,#2499));
#512=EDGE_LOOP('',(#2500,#2501));
#513=EDGE_LOOP('',(#2502,#2503,#2504,#2505));
#514=EDGE_LOOP('',(#2506,#2507));
#515=EDGE_LOOP('',(#2508,#2509,#2510,#2511,#2512));
#516=EDGE_LOOP('',(#2513));
#517=EDGE_LOOP('',(#2514));
#518=EDGE_LOOP('',(#2515,#2516,#2517,#2518));
#519=EDGE_LOOP('',(#2519));
#520=EDGE_LOOP('',(#2520));
#521=EDGE_LOOP('',(#2521,#2522,#2523,#2524));
#522=EDGE_LOOP('',(#2525));
#523=EDGE_LOOP('',(#2526));
#524=EDGE_LOOP('',(#2527));
#525=EDGE_LOOP('',(#2528));
#526=EDGE_LOOP('',(#2529,#2530,#2531,#2532));
#527=EDGE_LOOP('',(#2533,#2534,#2535,#2536));
#528=EDGE_LOOP('',(#2537,#2538,#2539,#2540));
#529=EDGE_LOOP('',(#2541,#2542,#2543,#2544));
#530=EDGE_LOOP('',(#2545));
#531=EDGE_LOOP('',(#2546));
#532=EDGE_LOOP('',(#2547,#2548,#2549,#2550));
#533=EDGE_LOOP('',(#2551));
#534=EDGE_LOOP('',(#2552));
#535=EDGE_LOOP('',(#2553));
#536=EDGE_LOOP('',(#2554));
#537=EDGE_LOOP('',(#2555));
#538=EDGE_LOOP('',(#2556));
#539=EDGE_LOOP('',(#2557,#2558,#2559,#2560,#2561));
#540=EDGE_LOOP('',(#2562,#2563,#2564,#2565,#2566));
#541=EDGE_LOOP('',(#2567,#2568,#2569,#2570,#2571));
#542=EDGE_LOOP('',(#2572,#2573,#2574,#2575,#2576));
#543=EDGE_LOOP('',(#2577));
#544=EDGE_LOOP('',(#2578));
#545=EDGE_LOOP('',(#2579,#2580,#2581,#2582));
#546=EDGE_LOOP('',(#2583,#2584,#2585,#2586));
#547=EDGE_LOOP('',(#2587));
#548=EDGE_LOOP('',(#2588));
#549=EDGE_LOOP('',(#2589));
#550=EDGE_LOOP('',(#2590));
#551=EDGE_LOOP('',(#2591,#2592,#2593,#2594));
#552=EDGE_LOOP('',(#2595));
#553=EDGE_LOOP('',(#2596));
#554=EDGE_LOOP('',(#2597,#2598,#2599,#2600,#2601,#2602,#2603,#2604));
#555=EDGE_LOOP('',(#2605,#2606,#2607,#2608,#2609,#2610,#2611,#2612));
#556=EDGE_LOOP('',(#2613,#2614,#2615,#2616));
#557=EDGE_LOOP('',(#2617));
#558=EDGE_LOOP('',(#2618,#2619,#2620,#2621));
#559=EDGE_LOOP('',(#2622,#2623,#2624,#2625));
#560=EDGE_LOOP('',(#2626,#2627,#2628,#2629,#2630,#2631,#2632));
#561=EDGE_LOOP('',(#2633,#2634,#2635,#2636,#2637,#2638,#2639));
#562=EDGE_LOOP('',(#2640,#2641,#2642,#2643));
#563=EDGE_LOOP('',(#2644,#2645,#2646,#2647));
#564=EDGE_LOOP('',(#2648,#2649,#2650,#2651));
#565=EDGE_LOOP('',(#2652,#2653,#2654,#2655));
#566=EDGE_LOOP('',(#2656,#2657,#2658,#2659));
#567=EDGE_LOOP('',(#2660,#2661,#2662,#2663));
#568=EDGE_LOOP('',(#2664));
#569=EDGE_LOOP('',(#2665,#2666,#2667,#2668));
#570=(
BOUNDED_CURVE()
B_SPLINE_CURVE(2,(#3913,#3914,#3915,#3916,#3917,#3918,#3919,#3920,#3921),
 .UNSPECIFIED.,.F.,.F.)
B_SPLINE_CURVE_WITH_KNOTS((3,2,2,2,3),(0.99,0.9925,0.995,0.9975,1.),
 .UNSPECIFIED.)
CURVE()
GEOMETRIC_REPRESENTATION_ITEM()
RATIONAL_B_SPLINE_CURVE((1.,0.923879532511287,1.,0.923879532511287,1.,0.923879532511287,
1.,0.923879532511287,1.))
REPRESENTATION_ITEM('')
);
#571=(
BOUNDED_CURVE()
B_SPLINE_CURVE(2,(#3924,#3925,#3926,#3927,#3928,#3929,#3930,#3931,#3932),
 .UNSPECIFIED.,.F.,.F.)
B_SPLINE_CURVE_WITH_KNOTS((3,2,2,2,3),(0.99,0.9925,0.995,0.9975,1.),
 .UNSPECIFIED.)
CURVE()
GEOMETRIC_REPRESENTATION_ITEM()
RATIONAL_B_SPLINE_CURVE((1.,0.923879532511287,1.,0.923879532511287,1.,0.923879532511287,
1.,0.923879532511287,1.))
REPRESENTATION_ITEM('')
);
#572=(
BOUNDED_CURVE()
B_SPLINE_CURVE(2,(#3937,#3938,#3939,#3940,#3941,#3942,#3943,#3944,#3945,
#3946,#3947,#3948,#3949,#3950,#3951,#3952,#3953),.UNSPECIFIED.,.F.,.F.)
B_SPLINE_CURVE_WITH_KNOTS((3,2,2,2,2,2,2,2,3),(0.97,0.9725,0.975,0.9775,
0.98,0.9825,0.985,0.9875,0.99),.UNSPECIFIED.)
CURVE()
GEOMETRIC_REPRESENTATION_ITEM()
RATIONAL_B_SPLINE_CURVE((1.,0.923879532511287,1.,0.923879532511287,1.,0.923879532511287,
1.,0.923879532511287,1.,0.923879532511287,1.,0.923879532511287,1.,0.923879532511287,
1.,0.923879532511287,1.))
REPRESENTATION_ITEM('')
);
#573=(
BOUNDED_CURVE()
B_SPLINE_CURVE(2,(#3954,#3955,#3956,#3957,#3958,#3959,#3960,#3961,#3962,
#3963,#3964,#3965,#3966,#3967,#3968,#3969,#3970),.UNSPECIFIED.,.F.,.F.)
B_SPLINE_CURVE_WITH_KNOTS((3,2,2,2,2,2,2,2,3),(0.97,0.9725,0.975,0.9775,
0.98,0.9825,0.985,0.9875,0.99),.UNSPECIFIED.)
CURVE()
GEOMETRIC_REPRESENTATION_ITEM()
RATIONAL_B_SPLINE_CURVE((1.,0.923879532511287,1.,0.923879532511287,1.,0.923879532511287,
1.,0.923879532511287,1.,0.923879532511287,1.,0.923879532511287,1.,0.923879532511287,
1.,0.923879532511287,1.))
REPRESENTATION_ITEM('')
);
#574=(
BOUNDED_CURVE()
B_SPLINE_CURVE(2,(#3975,#3976,#3977,#3978,#3979,#3980,#3981,#3982,#3983,
#3984,#3985,#3986,#3987,#3988,#3989,#3990,#3991),.UNSPECIFIED.,.F.,.F.)
B_SPLINE_CURVE_WITH_KNOTS((3,2,2,2,2,2,2,2,3),(0.95,0.9525,0.955,0.9575,
0.96,0.9625,0.965,0.9675,0.97),.UNSPECIFIED.)
CURVE()
GEOMETRIC_REPRESENTATION_ITEM()
RATIONAL_B_SPLINE_CURVE((1.,0.923879532511287,1.,0.923879532511287,1.,0.923879532511287,
1.,0.923879532511287,1.,0.923879532511287,1.,0.923879532511287,1.,0.923879532511287,
1.,0.923879532511287,1.))
REPRESENTATION_ITEM('')
);
#575=(
BOUNDED_CURVE()
B_SPLINE_CURVE(2,(#3992,#3993,#3994,#3995,#3996,#3997,#3998,#3999,#4000,
#4001,#4002,#4003,#4004,#4005,#4006,#4007,#4008),.UNSPECIFIED.,.F.,.F.)
B_SPLINE_CURVE_WITH_KNOTS((3,2,2,2,2,2,2,2,3),(0.95,0.9525,0.955,0.9575,
0.96,0.9625,0.965,0.9675,0.97),.UNSPECIFIED.)
CURVE()
GEOMETRIC_REPRESENTATION_ITEM()
RATIONAL_B_SPLINE_CURVE((1.,0.923879532511287,1.,0.923879532511287,1.,0.923879532511287,
1.,0.923879532511287,1.,0.923879532511287,1.,0.923879532511287,1.,0.923879532511287,
1.,0.923879532511287,1.))
REPRESENTATION_ITEM('')
);
#576=(
BOUNDED_CURVE()
B_SPLINE_CURVE(2,(#4013,#4014,#4015,#4016,#4017,#4018,#4019,#4020,#4021,
#4022,#4023,#4024,#4025,#4026,#4027,#4028,#4029),.UNSPECIFIED.,.F.,.F.)
B_SPLINE_CURVE_WITH_KNOTS((3,2,2,2,2,2,2,2,3),(0.93,0.9325,0.935,0.9375,
0.94,0.9425,0.945,0.9475,0.95),.UNSPECIFIED.)
CURVE()
GEOMETRIC_REPRESENTATION_ITEM()
RATIONAL_B_SPLINE_CURVE((1.,0.923879532511287,1.,0.923879532511287,1.,0.923879532511287,
1.,0.923879532511287,1.,0.923879532511287,1.,0.923879532511287,1.,0.923879532511287,
1.,0.923879532511287,1.))
REPRESENTATION_ITEM('')
);
#577=(
BOUNDED_CURVE()
B_SPLINE_CURVE(2,(#4030,#4031,#4032,#4033,#4034,#4035,#4036,#4037,#4038,
#4039,#4040,#4041,#4042,#4043,#4044,#4045,#4046),.UNSPECIFIED.,.F.,.F.)
B_SPLINE_CURVE_WITH_KNOTS((3,2,2,2,2,2,2,2,3),(0.93,0.9325,0.935,0.9375,
0.94,0.9425,0.945,0.9475,0.95),.UNSPECIFIED.)
CURVE()
GEOMETRIC_REPRESENTATION_ITEM()
RATIONAL_B_SPLINE_CURVE((1.,0.923879532511287,1.,0.923879532511287,1.,0.923879532511287,
1.,0.923879532511287,1.,0.923879532511287,1.,0.923879532511287,1.,0.923879532511287,
1.,0.923879532511287,1.))
REPRESENTATION_ITEM('')
);
#578=(
BOUNDED_CURVE()
B_SPLINE_CURVE(2,(#4051,#4052,#4053,#4054,#4055,#4056,#4057,#4058,#4059,
#4060,#4061,#4062,#4063,#4064,#4065,#4066,#4067),.UNSPECIFIED.,.F.,.F.)
B_SPLINE_CURVE_WITH_KNOTS((3,2,2,2,2,2,2,2,3),(0.91,0.9125,0.915,0.9175,
0.92,0.9225,0.925,0.9275,0.93),.UNSPECIFIED.)
CURVE()
GEOMETRIC_REPRESENTATION_ITEM()
RATIONAL_B_SPLINE_CURVE((1.,0.923879532511287,1.,0.923879532511287,1.,0.923879532511287,
1.,0.923879532511287,1.,0.923879532511287,1.,0.923879532511287,1.,0.923879532511287,
1.,0.923879532511287,1.))
REPRESENTATION_ITEM('')
);
#579=(
BOUNDED_CURVE()
B_SPLINE_CURVE(2,(#4068,#4069,#4070,#4071,#4072,#4073,#4074,#4075,#4076,
#4077,#4078,#4079,#4080,#4081,#4082,#4083,#4084),.UNSPECIFIED.,.F.,.F.)
B_SPLINE_CURVE_WITH_KNOTS((3,2,2,2,2,2,2,2,3),(0.91,0.9125,0.915,0.9175,
0.92,0.9225,0.925,0.9275,0.93),.UNSPECIFIED.)
CURVE()
GEOMETRIC_REPRESENTATION_ITEM()
RATIONAL_B_SPLINE_CURVE((1.,0.923879532511287,1.,0.923879532511287,1.,0.923879532511287,
1.,0.923879532511287,1.,0.923879532511287,1.,0.923879532511287,1.,0.923879532511287,
1.,0.923879532511287,1.))
REPRESENTATION_ITEM('')
);
#580=(
BOUNDED_CURVE()
B_SPLINE_CURVE(2,(#4089,#4090,#4091,#4092,#4093,#4094,#4095,#4096,#4097,
#4098,#4099,#4100,#4101,#4102,#4103,#4104,#4105),.UNSPECIFIED.,.F.,.F.)
B_SPLINE_CURVE_WITH_KNOTS((3,2,2,2,2,2,2,2,3),(0.89,0.8925,0.895,0.8975,
0.9,0.9025,0.905,0.9075,0.91),.UNSPECIFIED.)
CURVE()
GEOMETRIC_REPRESENTATION_ITEM()
RATIONAL_B_SPLINE_CURVE((1.,0.923879532511287,1.,0.923879532511287,1.,0.923879532511287,
1.,0.923879532511287,1.,0.923879532511287,1.,0.923879532511287,1.,0.923879532511287,
1.,0.923879532511287,1.))
REPRESENTATION_ITEM('')
);
#581=(
BOUNDED_CURVE()
B_SPLINE_CURVE(2,(#4106,#4107,#4108,#4109,#4110,#4111,#4112,#4113,#4114,
#4115,#4116,#4117,#4118,#4119,#4120,#4121,#4122),.UNSPECIFIED.,.F.,.F.)
B_SPLINE_CURVE_WITH_KNOTS((3,2,2,2,2,2,2,2,3),(0.89,0.8925,0.895,0.8975,
0.9,0.9025,0.905,0.9075,0.91),.UNSPECIFIED.)
CURVE()
GEOMETRIC_REPRESENTATION_ITEM()
RATIONAL_B_SPLINE_CURVE((1.,0.923879532511287,1.,0.923879532511287,1.,0.923879532511287,
1.,0.923879532511287,1.,0.923879532511287,1.,0.923879532511287,1.,0.923879532511287,
1.,0.923879532511287,1.))
REPRESENTATION_ITEM('')
);
#582=(
BOUNDED_CURVE()
B_SPLINE_CURVE(2,(#4127,#4128,#4129,#4130,#4131,#4132,#4133,#4134,#4135,
#4136,#4137,#4138,#4139,#4140,#4141,#4142,#4143),.UNSPECIFIED.,.F.,.F.)
B_SPLINE_CURVE_WITH_KNOTS((3,2,2,2,2,2,2,2,3),(0.87,0.8725,0.875,0.8775,
0.88,0.8825,0.885,0.8875,0.89),.UNSPECIFIED.)
CURVE()
GEOMETRIC_REPRESENTATION_ITEM()
RATIONAL_B_SPLINE_CURVE((1.,0.923879532511287,1.,0.923879532511287,1.,0.923879532511287,
1.,0.923879532511287,1.,0.923879532511287,1.,0.923879532511287,1.,0.923879532511287,
1.,0.923879532511287,1.))
REPRESENTATION_ITEM('')
);
#583=(
BOUNDED_CURVE()
B_SPLINE_CURVE(2,(#4144,#4145,#4146,#4147,#4148,#4149,#4150,#4151,#4152,
#4153,#4154,#4155,#4156,#4157,#4158,#4159,#4160),.UNSPECIFIED.,.F.,.F.)
B_SPLINE_CURVE_WITH_KNOTS((3,2,2,2,2,2,2,2,3),(0.87,0.8725,0.875,0.8775,
0.88,0.8825,0.885,0.8875,0.89),.UNSPECIFIED.)
CURVE()
GEOMETRIC_REPRESENTATION_ITEM()
RATIONAL_B_SPLINE_CURVE((1.,0.923879532511287,1.,0.923879532511287,1.,0.923879532511287,
1.,0.923879532511287,1.,0.923879532511287,1.,0.923879532511287,1.,0.923879532511287,
1.,0.923879532511287,1.))
REPRESENTATION_ITEM('')
);
#584=(
BOUNDED_CURVE()
B_SPLINE_CURVE(2,(#4165,#4166,#4167,#4168,#4169,#4170,#4171,#4172,#4173,
#4174,#4175,#4176,#4177,#4178,#4179,#4180,#4181),.UNSPECIFIED.,.F.,.F.)
B_SPLINE_CURVE_WITH_KNOTS((3,2,2,2,2,2,2,2,3),(0.85,0.8525,0.855,0.8575,
0.86,0.8625,0.865,0.8675,0.87),.UNSPECIFIED.)
CURVE()
GEOMETRIC_REPRESENTATION_ITEM()
RATIONAL_B_SPLINE_CURVE((1.,0.923879532511287,1.,0.923879532511287,1.,0.923879532511287,
1.,0.923879532511287,1.,0.923879532511287,1.,0.923879532511287,1.,0.923879532511287,
1.,0.923879532511287,1.))
REPRESENTATION_ITEM('')
);
#585=(
BOUNDED_CURVE()
B_SPLINE_CURVE(2,(#4182,#4183,#4184,#4185,#4186,#4187,#4188,#4189,#4190,
#4191,#4192,#4193,#4194,#4195,#4196,#4197,#4198),.UNSPECIFIED.,.F.,.F.)
B_SPLINE_CURVE_WITH_KNOTS((3,2,2,2,2,2,2,2,3),(0.85,0.8525,0.855,0.8575,
0.86,0.8625,0.865,0.8675,0.87),.UNSPECIFIED.)
CURVE()
GEOMETRIC_REPRESENTATION_ITEM()
RATIONAL_B_SPLINE_CURVE((1.,0.923879532511287,1.,0.923879532511287,1.,0.923879532511287,
1.,0.923879532511287,1.,0.923879532511287,1.,0.923879532511287,1.,0.923879532511287,
1.,0.923879532511287,1.))
REPRESENTATION_ITEM('')
);
#586=(
BOUNDED_CURVE()
B_SPLINE_CURVE(2,(#4203,#4204,#4205,#4206,#4207,#4208,#4209,#4210,#4211,
#4212,#4213,#4214,#4215,#4216,#4217,#4218,#4219),.UNSPECIFIED.,.F.,.F.)
B_SPLINE_CURVE_WITH_KNOTS((3,2,2,2,2,2,2,2,3),(0.83,0.8325,0.835,0.8375,
0.84,0.8425,0.845,0.8475,0.85),.UNSPECIFIED.)
CURVE()
GEOMETRIC_REPRESENTATION_ITEM()
RATIONAL_B_SPLINE_CURVE((1.,0.923879532511287,1.,0.923879532511287,1.,0.923879532511287,
1.,0.923879532511287,1.,0.923879532511287,1.,0.923879532511287,1.,0.923879532511287,
1.,0.923879532511287,1.))
REPRESENTATION_ITEM('')
);
#587=(
BOUNDED_CURVE()
B_SPLINE_CURVE(2,(#4220,#4221,#4222,#4223,#4224,#4225,#4226,#4227,#4228,
#4229,#4230,#4231,#4232,#4233,#4234,#4235,#4236),.UNSPECIFIED.,.F.,.F.)
B_SPLINE_CURVE_WITH_KNOTS((3,2,2,2,2,2,2,2,3),(0.83,0.8325,0.835,0.8375,
0.84,0.8425,0.845,0.8475,0.85),.UNSPECIFIED.)
CURVE()
GEOMETRIC_REPRESENTATION_ITEM()
RATIONAL_B_SPLINE_CURVE((1.,0.923879532511287,1.,0.923879532511287,1.,0.923879532511287,
1.,0.923879532511287,1.,0.923879532511287,1.,0.923879532511287,1.,0.923879532511287,
1.,0.923879532511287,1.))
REPRESENTATION_ITEM('')
);
#588=(
BOUNDED_CURVE()
B_SPLINE_CURVE(2,(#4241,#4242,#4243,#4244,#4245,#4246,#4247,#4248,#4249,
#4250,#4251,#4252,#4253,#4254,#4255,#4256,#4257),.UNSPECIFIED.,.F.,.F.)
B_SPLINE_CURVE_WITH_KNOTS((3,2,2,2,2,2,2,2,3),(0.81,0.8125,0.815,0.8175,
0.82,0.8225,0.825,0.8275,0.83),.UNSPECIFIED.)
CURVE()
GEOMETRIC_REPRESENTATION_ITEM()
RATIONAL_B_SPLINE_CURVE((1.,0.923879532511287,1.,0.923879532511287,1.,0.923879532511287,
1.,0.923879532511287,1.,0.923879532511287,1.,0.923879532511287,1.,0.923879532511287,
1.,0.923879532511287,1.))
REPRESENTATION_ITEM('')
);
#589=(
BOUNDED_CURVE()
B_SPLINE_CURVE(2,(#4258,#4259,#4260,#4261,#4262,#4263,#4264,#4265,#4266,
#4267,#4268,#4269,#4270,#4271,#4272,#4273,#4274),.UNSPECIFIED.,.F.,.F.)
B_SPLINE_CURVE_WITH_KNOTS((3,2,2,2,2,2,2,2,3),(0.81,0.8125,0.815,0.8175,
0.82,0.8225,0.825,0.8275,0.83),.UNSPECIFIED.)
CURVE()
GEOMETRIC_REPRESENTATION_ITEM()
RATIONAL_B_SPLINE_CURVE((1.,0.923879532511287,1.,0.923879532511287,1.,0.923879532511287,
1.,0.923879532511287,1.,0.923879532511287,1.,0.923879532511287,1.,0.923879532511287,
1.,0.923879532511287,1.))
REPRESENTATION_ITEM('')
);
#590=(
BOUNDED_CURVE()
B_SPLINE_CURVE(2,(#4279,#4280,#4281,#4282,#4283,#4284,#4285,#4286,#4287,
#4288,#4289,#4290,#4291,#4292,#4293,#4294,#4295),.UNSPECIFIED.,.F.,.F.)
B_SPLINE_CURVE_WITH_KNOTS((3,2,2,2,2,2,2,2,3),(0.79,0.7925,0.795,0.7975,
0.8,0.8025,0.805,0.8075,0.81),.UNSPECIFIED.)
CURVE()
GEOMETRIC_REPRESENTATION_ITEM()
RATIONAL_B_SPLINE_CURVE((1.,0.923879532511287,1.,0.923879532511287,1.,0.923879532511287,
1.,0.923879532511287,1.,0.923879532511287,1.,0.923879532511287,1.,0.923879532511287,
1.,0.923879532511287,1.))
REPRESENTATION_ITEM('')
);
#591=(
BOUNDED_CURVE()
B_SPLINE_CURVE(2,(#4296,#4297,#4298,#4299,#4300,#4301,#4302,#4303,#4304,
#4305,#4306,#4307,#4308,#4309,#4310,#4311,#4312),.UNSPECIFIED.,.F.,.F.)
B_SPLINE_CURVE_WITH_KNOTS((3,2,2,2,2,2,2,2,3),(0.79,0.7925,0.795,0.7975,
0.8,0.8025,0.805,0.8075,0.81),.UNSPECIFIED.)
CURVE()
GEOMETRIC_REPRESENTATION_ITEM()
RATIONAL_B_SPLINE_CURVE((1.,0.923879532511287,1.,0.923879532511287,1.,0.923879532511287,
1.,0.923879532511287,1.,0.923879532511287,1.,0.923879532511287,1.,0.923879532511287,
1.,0.923879532511287,1.))
REPRESENTATION_ITEM('')
);
#592=(
BOUNDED_CURVE()
B_SPLINE_CURVE(2,(#4317,#4318,#4319,#4320,#4321,#4322,#4323,#4324,#4325,
#4326,#4327,#4328,#4329,#4330,#4331,#4332,#4333),.UNSPECIFIED.,.F.,.F.)
B_SPLINE_CURVE_WITH_KNOTS((3,2,2,2,2,2,2,2,3),(0.77,0.7725,0.775,0.7775,
0.78,0.7825,0.785,0.7875,0.79),.UNSPECIFIED.)
CURVE()
GEOMETRIC_REPRESENTATION_ITEM()
RATIONAL_B_SPLINE_CURVE((1.,0.923879532511287,1.,0.923879532511287,1.,0.923879532511287,
1.,0.923879532511287,1.,0.923879532511287,1.,0.923879532511287,1.,0.923879532511287,
1.,0.923879532511287,1.))
REPRESENTATION_ITEM('')
);
#593=(
BOUNDED_CURVE()
B_SPLINE_CURVE(2,(#4334,#4335,#4336,#4337,#4338,#4339,#4340,#4341,#4342,
#4343,#4344,#4345,#4346,#4347,#4348,#4349,#4350),.UNSPECIFIED.,.F.,.F.)
B_SPLINE_CURVE_WITH_KNOTS((3,2,2,2,2,2,2,2,3),(0.77,0.7725,0.775,0.7775,
0.78,0.7825,0.785,0.7875,0.79),.UNSPECIFIED.)
CURVE()
GEOMETRIC_REPRESENTATION_ITEM()
RATIONAL_B_SPLINE_CURVE((1.,0.923879532511287,1.,0.923879532511287,1.,0.923879532511287,
1.,0.923879532511287,1.,0.923879532511287,1.,0.923879532511287,1.,0.923879532511287,
1.,0.923879532511287,1.))
REPRESENTATION_ITEM('')
);
#594=(
BOUNDED_CURVE()
B_SPLINE_CURVE(2,(#4355,#4356,#4357,#4358,#4359,#4360,#4361,#4362,#4363,
#4364,#4365,#4366,#4367,#4368,#4369,#4370,#4371),.UNSPECIFIED.,.F.,.F.)
B_SPLINE_CURVE_WITH_KNOTS((3,2,2,2,2,2,2,2,3),(0.75,0.7525,0.755,0.7575,
0.76,0.7625,0.765,0.7675,0.77),.UNSPECIFIED.)
CURVE()
GEOMETRIC_REPRESENTATION_ITEM()
RATIONAL_B_SPLINE_CURVE((1.,0.923879532511287,1.,0.923879532511287,1.,0.923879532511287,
1.,0.923879532511287,1.,0.923879532511287,1.,0.923879532511287,1.,0.923879532511287,
1.,0.923879532511287,1.))
REPRESENTATION_ITEM('')
);
#595=(
BOUNDED_CURVE()
B_SPLINE_CURVE(2,(#4372,#4373,#4374,#4375,#4376,#4377,#4378,#4379,#4380,
#4381,#4382,#4383,#4384,#4385,#4386,#4387,#4388),.UNSPECIFIED.,.F.,.F.)
B_SPLINE_CURVE_WITH_KNOTS((3,2,2,2,2,2,2,2,3),(0.75,0.7525,0.755,0.7575,
0.76,0.7625,0.765,0.7675,0.77),.UNSPECIFIED.)
CURVE()
GEOMETRIC_REPRESENTATION_ITEM()
RATIONAL_B_SPLINE_CURVE((1.,0.923879532511287,1.,0.923879532511287,1.,0.923879532511287,
1.,0.923879532511287,1.,0.923879532511287,1.,0.923879532511287,1.,0.923879532511287,
1.,0.923879532511287,1.))
REPRESENTATION_ITEM('')
);
#596=(
BOUNDED_CURVE()
B_SPLINE_CURVE(2,(#4393,#4394,#4395,#4396,#4397,#4398,#4399,#4400,#4401,
#4402,#4403,#4404,#4405,#4406,#4407,#4408,#4409),.UNSPECIFIED.,.F.,.F.)
B_SPLINE_CURVE_WITH_KNOTS((3,2,2,2,2,2,2,2,3),(0.73,0.7325,0.735,0.7375,
0.74,0.7425,0.745,0.7475,0.75),.UNSPECIFIED.)
CURVE()
GEOMETRIC_REPRESENTATION_ITEM()
RATIONAL_B_SPLINE_CURVE((1.,0.923879532511287,1.,0.923879532511287,1.,0.923879532511287,
1.,0.923879532511287,1.,0.923879532511287,1.,0.923879532511287,1.,0.923879532511287,
1.,0.923879532511287,1.))
REPRESENTATION_ITEM('')
);
#597=(
BOUNDED_CURVE()
B_SPLINE_CURVE(2,(#4410,#4411,#4412,#4413,#4414,#4415,#4416,#4417,#4418,
#4419,#4420,#4421,#4422,#4423,#4424,#4425,#4426),.UNSPECIFIED.,.F.,.F.)
B_SPLINE_CURVE_WITH_KNOTS((3,2,2,2,2,2,2,2,3),(0.73,0.7325,0.735,0.7375,
0.74,0.7425,0.745,0.7475,0.75),.UNSPECIFIED.)
CURVE()
GEOMETRIC_REPRESENTATION_ITEM()
RATIONAL_B_SPLINE_CURVE((1.,0.923879532511287,1.,0.923879532511287,1.,0.923879532511287,
1.,0.923879532511287,1.,0.923879532511287,1.,0.923879532511287,1.,0.923879532511287,
1.,0.923879532511287,1.))
REPRESENTATION_ITEM('')
);
#598=(
BOUNDED_CURVE()
B_SPLINE_CURVE(2,(#4431,#4432,#4433,#4434,#4435,#4436,#4437,#4438,#4439,
#4440,#4441,#4442,#4443,#4444,#4445,#4446,#4447),.UNSPECIFIED.,.F.,.F.)
B_SPLINE_CURVE_WITH_KNOTS((3,2,2,2,2,2,2,2,3),(0.71,0.7125,0.715,0.7175,
0.72,0.7225,0.725,0.7275,0.73),.UNSPECIFIED.)
CURVE()
GEOMETRIC_REPRESENTATION_ITEM()
RATIONAL_B_SPLINE_CURVE((1.,0.923879532511287,1.,0.923879532511287,1.,0.923879532511287,
1.,0.923879532511287,1.,0.923879532511287,1.,0.923879532511287,1.,0.923879532511287,
1.,0.923879532511287,1.))
REPRESENTATION_ITEM('')
);
#599=(
BOUNDED_CURVE()
B_SPLINE_CURVE(2,(#4448,#4449,#4450,#4451,#4452,#4453,#4454,#4455,#4456,
#4457,#4458,#4459,#4460,#4461,#4462,#4463,#4464),.UNSPECIFIED.,.F.,.F.)
B_SPLINE_CURVE_WITH_KNOTS((3,2,2,2,2,2,2,2,3),(0.71,0.7125,0.715,0.7175,
0.72,0.7225,0.725,0.7275,0.73),.UNSPECIFIED.)
CURVE()
GEOMETRIC_REPRESENTATION_ITEM()
RATIONAL_B_SPLINE_CURVE((1.,0.923879532511287,1.,0.923879532511287,1.,0.923879532511287,
1.,0.923879532511287,1.,0.923879532511287,1.,0.923879532511287,1.,0.923879532511287,
1.,0.923879532511287,1.))
REPRESENTATION_ITEM('')
);
#600=(
BOUNDED_CURVE()
B_SPLINE_CURVE(2,(#4469,#4470,#4471,#4472,#4473,#4474,#4475,#4476,#4477,
#4478,#4479,#4480,#4481,#4482,#4483,#4484,#4485),.UNSPECIFIED.,.F.,.F.)
B_SPLINE_CURVE_WITH_KNOTS((3,2,2,2,2,2,2,2,3),(0.69,0.6925,0.695,0.6975,
0.7,0.7025,0.705,0.7075,0.71),.UNSPECIFIED.)
CURVE()
GEOMETRIC_REPRESENTATION_ITEM()
RATIONAL_B_SPLINE_CURVE((1.,0.923879532511287,1.,0.923879532511287,1.,0.923879532511287,
1.,0.923879532511287,1.,0.923879532511287,1.,0.923879532511287,1.,0.923879532511287,
1.,0.923879532511287,1.))
REPRESENTATION_ITEM('')
);
#601=(
BOUNDED_CURVE()
B_SPLINE_CURVE(2,(#4486,#4487,#4488,#4489,#4490,#4491,#4492,#4493,#4494,
#4495,#4496,#4497,#4498,#4499,#4500,#4501,#4502),.UNSPECIFIED.,.F.,.F.)
B_SPLINE_CURVE_WITH_KNOTS((3,2,2,2,2,2,2,2,3),(0.69,0.6925,0.695,0.6975,
0.7,0.7025,0.705,0.7075,0.71),.UNSPECIFIED.)
CURVE()
GEOMETRIC_REPRESENTATION_ITEM()
RATIONAL_B_SPLINE_CURVE((1.,0.923879532511287,1.,0.923879532511287,1.,0.923879532511287,
1.,0.923879532511287,1.,0.923879532511287,1.,0.923879532511287,1.,0.923879532511287,
1.,0.923879532511287,1.))
REPRESENTATION_ITEM('')
);
#602=(
BOUNDED_CURVE()
B_SPLINE_CURVE(2,(#4507,#4508,#4509,#4510,#4511,#4512,#4513,#4514,#4515,
#4516,#4517,#4518,#4519,#4520,#4521,#4522,#4523),.UNSPECIFIED.,.F.,.F.)
B_SPLINE_CURVE_WITH_KNOTS((3,2,2,2,2,2,2,2,3),(0.67,0.6725,0.675,0.6775,
0.68,0.6825,0.685,0.6875,0.69),.UNSPECIFIED.)
CURVE()
GEOMETRIC_REPRESENTATION_ITEM()
RATIONAL_B_SPLINE_CURVE((1.,0.923879532511287,1.,0.923879532511287,1.,0.923879532511287,
1.,0.923879532511287,1.,0.923879532511287,1.,0.923879532511287,1.,0.923879532511287,
1.,0.923879532511287,1.))
REPRESENTATION_ITEM('')
);
#603=(
BOUNDED_CURVE()
B_SPLINE_CURVE(2,(#4524,#4525,#4526,#4527,#4528,#4529,#4530,#4531,#4532,
#4533,#4534,#4535,#4536,#4537,#4538,#4539,#4540),.UNSPECIFIED.,.F.,.F.)
B_SPLINE_CURVE_WITH_KNOTS((3,2,2,2,2,2,2,2,3),(0.67,0.6725,0.675,0.6775,
0.68,0.6825,0.685,0.6875,0.69),.UNSPECIFIED.)
CURVE()
GEOMETRIC_REPRESENTATION_ITEM()
RATIONAL_B_SPLINE_CURVE((1.,0.923879532511287,1.,0.923879532511287,1.,0.923879532511287,
1.,0.923879532511287,1.,0.923879532511287,1.,0.923879532511287,1.,0.923879532511287,
1.,0.923879532511287,1.))
REPRESENTATION_ITEM('')
);
#604=(
BOUNDED_CURVE()
B_SPLINE_CURVE(2,(#4545,#4546,#4547,#4548,#4549,#4550,#4551,#4552,#4553,
#4554,#4555,#4556,#4557,#4558,#4559,#4560,#4561),.UNSPECIFIED.,.F.,.F.)
B_SPLINE_CURVE_WITH_KNOTS((3,2,2,2,2,2,2,2,3),(0.65,0.6525,0.655,0.6575,
0.66,0.6625,0.665,0.6675,0.67),.UNSPECIFIED.)
CURVE()
GEOMETRIC_REPRESENTATION_ITEM()
RATIONAL_B_SPLINE_CURVE((1.,0.923879532511287,1.,0.923879532511287,1.,0.923879532511287,
1.,0.923879532511287,1.,0.923879532511287,1.,0.923879532511287,1.,0.923879532511287,
1.,0.923879532511287,1.))
REPRESENTATION_ITEM('')
);
#605=(
BOUNDED_CURVE()
B_SPLINE_CURVE(2,(#4562,#4563,#4564,#4565,#4566,#4567,#4568,#4569,#4570,
#4571,#4572,#4573,#4574,#4575,#4576,#4577,#4578),.UNSPECIFIED.,.F.,.F.)
B_SPLINE_CURVE_WITH_KNOTS((3,2,2,2,2,2,2,2,3),(0.65,0.6525,0.655,0.6575,
0.66,0.6625,0.665,0.6675,0.67),.UNSPECIFIED.)
CURVE()
GEOMETRIC_REPRESENTATION_ITEM()
RATIONAL_B_SPLINE_CURVE((1.,0.923879532511287,1.,0.923879532511287,1.,0.923879532511287,
1.,0.923879532511287,1.,0.923879532511287,1.,0.923879532511287,1.,0.923879532511287,
1.,0.923879532511287,1.))
REPRESENTATION_ITEM('')
);
#606=(
BOUNDED_CURVE()
B_SPLINE_CURVE(2,(#4583,#4584,#4585,#4586,#4587,#4588,#4589,#4590,#4591,
#4592,#4593,#4594,#4595,#4596,#4597,#4598,#4599),.UNSPECIFIED.,.F.,.F.)
B_SPLINE_CURVE_WITH_KNOTS((3,2,2,2,2,2,2,2,3),(0.63,0.6325,0.635,0.6375,
0.64,0.6425,0.645,0.6475,0.65),.UNSPECIFIED.)
CURVE()
GEOMETRIC_REPRESENTATION_ITEM()
RATIONAL_B_SPLINE_CURVE((1.,0.923879532511287,1.,0.923879532511287,1.,0.923879532511287,
1.,0.923879532511287,1.,0.923879532511287,1.,0.923879532511287,1.,0.923879532511287,
1.,0.923879532511287,1.))
REPRESENTATION_ITEM('')
);
#607=(
BOUNDED_CURVE()
B_SPLINE_CURVE(2,(#4600,#4601,#4602,#4603,#4604,#4605,#4606,#4607,#4608,
#4609,#4610,#4611,#4612,#4613,#4614,#4615,#4616),.UNSPECIFIED.,.F.,.F.)
B_SPLINE_CURVE_WITH_KNOTS((3,2,2,2,2,2,2,2,3),(0.63,0.6325,0.635,0.6375,
0.64,0.6425,0.645,0.6475,0.65),.UNSPECIFIED.)
CURVE()
GEOMETRIC_REPRESENTATION_ITEM()
RATIONAL_B_SPLINE_CURVE((1.,0.923879532511287,1.,0.923879532511287,1.,0.923879532511287,
1.,0.923879532511287,1.,0.923879532511287,1.,0.923879532511287,1.,0.923879532511287,
1.,0.923879532511287,1.))
REPRESENTATION_ITEM('')
);
#608=(
BOUNDED_CURVE()
B_SPLINE_CURVE(2,(#4621,#4622,#4623,#4624,#4625,#4626,#4627,#4628,#4629,
#4630,#4631,#4632,#4633,#4634,#4635,#4636,#4637),.UNSPECIFIED.,.F.,.F.)
B_SPLINE_CURVE_WITH_KNOTS((3,2,2,2,2,2,2,2,3),(0.61,0.6125,0.615,0.6175,
0.62,0.6225,0.625,0.6275,0.63),.UNSPECIFIED.)
CURVE()
GEOMETRIC_REPRESENTATION_ITEM()
RATIONAL_B_SPLINE_CURVE((1.,0.923879532511287,1.,0.923879532511287,1.,0.923879532511287,
1.,0.923879532511287,1.,0.923879532511287,1.,0.923879532511287,1.,0.923879532511287,
1.,0.923879532511287,1.))
REPRESENTATION_ITEM('')
);
#609=(
BOUNDED_CURVE()
B_SPLINE_CURVE(2,(#4638,#4639,#4640,#4641,#4642,#4643,#4644,#4645,#4646,
#4647,#4648,#4649,#4650,#4651,#4652,#4653,#4654),.UNSPECIFIED.,.F.,.F.)
B_SPLINE_CURVE_WITH_KNOTS((3,2,2,2,2,2,2,2,3),(0.61,0.6125,0.615,0.6175,
0.62,0.6225,0.625,0.6275,0.63),.UNSPECIFIED.)
CURVE()
GEOMETRIC_REPRESENTATION_ITEM()
RATIONAL_B_SPLINE_CURVE((1.,0.923879532511287,1.,0.923879532511287,1.,0.923879532511287,
1.,0.923879532511287,1.,0.923879532511287,1.,0.923879532511287,1.,0.923879532511287,
1.,0.923879532511287,1.))
REPRESENTATION_ITEM('')
);
#610=(
BOUNDED_CURVE()
B_SPLINE_CURVE(2,(#4659,#4660,#4661,#4662,#4663,#4664,#4665,#4666,#4667,
#4668,#4669,#4670,#4671,#4672,#4673,#4674,#4675),.UNSPECIFIED.,.F.,.F.)
B_SPLINE_CURVE_WITH_KNOTS((3,2,2,2,2,2,2,2,3),(0.59,0.5925,0.595,0.5975,
0.6,0.6025,0.605,0.6075,0.61),.UNSPECIFIED.)
CURVE()
GEOMETRIC_REPRESENTATION_ITEM()
RATIONAL_B_SPLINE_CURVE((1.,0.923879532511287,1.,0.923879532511287,1.,0.923879532511287,
1.,0.923879532511287,1.,0.923879532511287,1.,0.923879532511287,1.,0.923879532511287,
1.,0.923879532511287,1.))
REPRESENTATION_ITEM('')
);
#611=(
BOUNDED_CURVE()
B_SPLINE_CURVE(2,(#4676,#4677,#4678,#4679,#4680,#4681,#4682,#4683,#4684,
#4685,#4686,#4687,#4688,#4689,#4690,#4691,#4692),.UNSPECIFIED.,.F.,.F.)
B_SPLINE_CURVE_WITH_KNOTS((3,2,2,2,2,2,2,2,3),(0.59,0.5925,0.595,0.5975,
0.6,0.6025,0.605,0.6075,0.61),.UNSPECIFIED.)
CURVE()
GEOMETRIC_REPRESENTATION_ITEM()
RATIONAL_B_SPLINE_CURVE((1.,0.923879532511287,1.,0.923879532511287,1.,0.923879532511287,
1.,0.923879532511287,1.,0.923879532511287,1.,0.923879532511287,1.,0.923879532511287,
1.,0.923879532511287,1.))
REPRESENTATION_ITEM('')
);
#612=(
BOUNDED_CURVE()
B_SPLINE_CURVE(2,(#4697,#4698,#4699,#4700,#4701,#4702,#4703,#4704,#4705,
#4706,#4707,#4708,#4709,#4710,#4711,#4712,#4713),.UNSPECIFIED.,.F.,.F.)
B_SPLINE_CURVE_WITH_KNOTS((3,2,2,2,2,2,2,2,3),(0.57,0.5725,0.575,0.5775,
0.58,0.5825,0.585,0.5875,0.59),.UNSPECIFIED.)
CURVE()
GEOMETRIC_REPRESENTATION_ITEM()
RATIONAL_B_SPLINE_CURVE((1.,0.923879532511287,1.,0.923879532511287,1.,0.923879532511287,
1.,0.923879532511287,1.,0.923879532511287,1.,0.923879532511287,1.,0.923879532511287,
1.,0.923879532511287,1.))
REPRESENTATION_ITEM('')
);
#613=(
BOUNDED_CURVE()
B_SPLINE_CURVE(2,(#4714,#4715,#4716,#4717,#4718,#4719,#4720,#4721,#4722,
#4723,#4724,#4725,#4726,#4727,#4728,#4729,#4730),.UNSPECIFIED.,.F.,.F.)
B_SPLINE_CURVE_WITH_KNOTS((3,2,2,2,2,2,2,2,3),(0.57,0.5725,0.575,0.5775,
0.58,0.5825,0.585,0.5875,0.59),.UNSPECIFIED.)
CURVE()
GEOMETRIC_REPRESENTATION_ITEM()
RATIONAL_B_SPLINE_CURVE((1.,0.923879532511287,1.,0.923879532511287,1.,0.923879532511287,
1.,0.923879532511287,1.,0.923879532511287,1.,0.923879532511287,1.,0.923879532511287,
1.,0.923879532511287,1.))
REPRESENTATION_ITEM('')
);
#614=(
BOUNDED_CURVE()
B_SPLINE_CURVE(2,(#4735,#4736,#4737,#4738,#4739,#4740,#4741,#4742,#4743,
#4744,#4745,#4746,#4747,#4748,#4749,#4750,#4751),.UNSPECIFIED.,.F.,.F.)
B_SPLINE_CURVE_WITH_KNOTS((3,2,2,2,2,2,2,2,3),(0.55,0.5525,0.555,0.5575,
0.56,0.5625,0.565,0.5675,0.57),.UNSPECIFIED.)
CURVE()
GEOMETRIC_REPRESENTATION_ITEM()
RATIONAL_B_SPLINE_CURVE((1.,0.923879532511287,1.,0.923879532511287,1.,0.923879532511287,
1.,0.923879532511287,1.,0.923879532511287,1.,0.923879532511287,1.,0.923879532511287,
1.,0.923879532511287,1.))
REPRESENTATION_ITEM('')
);
#615=(
BOUNDED_CURVE()
B_SPLINE_CURVE(2,(#4752,#4753,#4754,#4755,#4756,#4757,#4758,#4759,#4760,
#4761,#4762,#4763,#4764,#4765,#4766,#4767,#4768),.UNSPECIFIED.,.F.,.F.)
B_SPLINE_CURVE_WITH_KNOTS((3,2,2,2,2,2,2,2,3),(0.55,0.5525,0.555,0.5575,
0.56,0.5625,0.565,0.5675,0.57),.UNSPECIFIED.)
CURVE()
GEOMETRIC_REPRESENTATION_ITEM()
RATIONAL_B_SPLINE_CURVE((1.,0.923879532511287,1.,0.923879532511287,1.,0.923879532511287,
1.,0.923879532511287,1.,0.923879532511287,1.,0.923879532511287,1.,0.923879532511287,
1.,0.923879532511287,1.))
REPRESENTATION_ITEM('')
);
#616=(
BOUNDED_CURVE()
B_SPLINE_CURVE(2,(#4773,#4774,#4775,#4776,#4777,#4778,#4779,#4780,#4781,
#4782,#4783,#4784,#4785,#4786,#4787,#4788,#4789),.UNSPECIFIED.,.F.,.F.)
B_SPLINE_CURVE_WITH_KNOTS((3,2,2,2,2,2,2,2,3),(0.53,0.5325,0.535,0.5375,
0.54,0.5425,0.545,0.5475,0.55),.UNSPECIFIED.)
CURVE()
GEOMETRIC_REPRESENTATION_ITEM()
RATIONAL_B_SPLINE_CURVE((1.,0.923879532511287,1.,0.923879532511287,1.,0.923879532511287,
1.,0.923879532511287,1.,0.923879532511287,1.,0.923879532511287,1.,0.923879532511287,
1.,0.923879532511287,1.))
REPRESENTATION_ITEM('')
);
#617=(
BOUNDED_CURVE()
B_SPLINE_CURVE(2,(#4790,#4791,#4792,#4793,#4794,#4795,#4796,#4797,#4798,
#4799,#4800,#4801,#4802,#4803,#4804,#4805,#4806),.UNSPECIFIED.,.F.,.F.)
B_SPLINE_CURVE_WITH_KNOTS((3,2,2,2,2,2,2,2,3),(0.53,0.5325,0.535,0.5375,
0.54,0.5425,0.545,0.5475,0.55),.UNSPECIFIED.)
CURVE()
GEOMETRIC_REPRESENTATION_ITEM()
RATIONAL_B_SPLINE_CURVE((1.,0.923879532511287,1.,0.923879532511287,1.,0.923879532511287,
1.,0.923879532511287,1.,0.923879532511287,1.,0.923879532511287,1.,0.923879532511287,
1.,0.923879532511287,1.))
REPRESENTATION_ITEM('')
);
#618=(
BOUNDED_CURVE()
B_SPLINE_CURVE(2,(#4811,#4812,#4813,#4814,#4815,#4816,#4817,#4818,#4819,
#4820,#4821,#4822,#4823,#4824,#4825,#4826,#4827),.UNSPECIFIED.,.F.,.F.)
B_SPLINE_CURVE_WITH_KNOTS((3,2,2,2,2,2,2,2,3),(0.51,0.5125,0.515,0.5175,
0.52,0.5225,0.525,0.5275,0.53),.UNSPECIFIED.)
CURVE()
GEOMETRIC_REPRESENTATION_ITEM()
RATIONAL_B_SPLINE_CURVE((1.,0.923879532511287,1.,0.923879532511287,1.,0.923879532511287,
1.,0.923879532511287,1.,0.923879532511287,1.,0.923879532511287,1.,0.923879532511287,
1.,0.923879532511287,1.))
REPRESENTATION_ITEM('')
);
#619=(
BOUNDED_CURVE()
B_SPLINE_CURVE(2,(#4828,#4829,#4830,#4831,#4832,#4833,#4834,#4835,#4836,
#4837,#4838,#4839,#4840,#4841,#4842,#4843,#4844),.UNSPECIFIED.,.F.,.F.)
B_SPLINE_CURVE_WITH_KNOTS((3,2,2,2,2,2,2,2,3),(0.51,0.5125,0.515,0.5175,
0.52,0.5225,0.525,0.5275,0.53),.UNSPECIFIED.)
CURVE()
GEOMETRIC_REPRESENTATION_ITEM()
RATIONAL_B_SPLINE_CURVE((1.,0.923879532511287,1.,0.923879532511287,1.,0.923879532511287,
1.,0.923879532511287,1.,0.923879532511287,1.,0.923879532511287,1.,0.923879532511287,
1.,0.923879532511287,1.))
REPRESENTATION_ITEM('')
);
#620=(
BOUNDED_CURVE()
B_SPLINE_CURVE(2,(#4849,#4850,#4851,#4852,#4853,#4854,#4855,#4856,#4857,
#4858,#4859,#4860,#4861,#4862,#4863,#4864,#4865),.UNSPECIFIED.,.F.,.F.)
B_SPLINE_CURVE_WITH_KNOTS((3,2,2,2,2,2,2,2,3),(0.49,0.4925,0.495,0.4975,
0.5,0.5025,0.505,0.5075,0.51),.UNSPECIFIED.)
CURVE()
GEOMETRIC_REPRESENTATION_ITEM()
RATIONAL_B_SPLINE_CURVE((1.,0.923879532511287,1.,0.923879532511287,1.,0.923879532511287,
1.,0.923879532511287,1.,0.923879532511287,1.,0.923879532511287,1.,0.923879532511287,
1.,0.923879532511287,1.))
REPRESENTATION_ITEM('')
);
#621=(
BOUNDED_CURVE()
B_SPLINE_CURVE(2,(#4866,#4867,#4868,#4869,#4870,#4871,#4872,#4873,#4874,
#4875,#4876,#4877,#4878,#4879,#4880,#4881,#4882),.UNSPECIFIED.,.F.,.F.)
B_SPLINE_CURVE_WITH_KNOTS((3,2,2,2,2,2,2,2,3),(0.49,0.4925,0.495,0.4975,
0.5,0.5025,0.505,0.5075,0.51),.UNSPECIFIED.)
CURVE()
GEOMETRIC_REPRESENTATION_ITEM()
RATIONAL_B_SPLINE_CURVE((1.,0.923879532511287,1.,0.923879532511287,1.,0.923879532511287,
1.,0.923879532511287,1.,0.923879532511287,1.,0.923879532511287,1.,0.923879532511287,
1.,0.923879532511287,1.))
REPRESENTATION_ITEM('')
);
#622=(
BOUNDED_CURVE()
B_SPLINE_CURVE(2,(#4887,#4888,#4889,#4890,#4891,#4892,#4893,#4894,#4895,
#4896,#4897,#4898,#4899,#4900,#4901,#4902,#4903),.UNSPECIFIED.,.F.,.F.)
B_SPLINE_CURVE_WITH_KNOTS((3,2,2,2,2,2,2,2,3),(0.47,0.4725,0.475,0.4775,
0.48,0.4825,0.485,0.4875,0.49),.UNSPECIFIED.)
CURVE()
GEOMETRIC_REPRESENTATION_ITEM()
RATIONAL_B_SPLINE_CURVE((1.,0.923879532511287,1.,0.923879532511287,1.,0.923879532511287,
1.,0.923879532511287,1.,0.923879532511287,1.,0.923879532511287,1.,0.923879532511287,
1.,0.923879532511287,1.))
REPRESENTATION_ITEM('')
);
#623=(
BOUNDED_CURVE()
B_SPLINE_CURVE(2,(#4904,#4905,#4906,#4907,#4908,#4909,#4910,#4911,#4912,
#4913,#4914,#4915,#4916,#4917,#4918,#4919,#4920),.UNSPECIFIED.,.F.,.F.)
B_SPLINE_CURVE_WITH_KNOTS((3,2,2,2,2,2,2,2,3),(0.47,0.4725,0.475,0.4775,
0.48,0.4825,0.485,0.4875,0.49),.UNSPECIFIED.)
CURVE()
GEOMETRIC_REPRESENTATION_ITEM()
RATIONAL_B_SPLINE_CURVE((1.,0.923879532511287,1.,0.923879532511287,1.,0.923879532511287,
1.,0.923879532511287,1.,0.923879532511287,1.,0.923879532511287,1.,0.923879532511287,
1.,0.923879532511287,1.))
REPRESENTATION_ITEM('')
);
#624=(
BOUNDED_CURVE()
B_SPLINE_CURVE(2,(#4925,#4926,#4927,#4928,#4929,#4930,#4931,#4932,#4933,
#4934,#4935,#4936,#4937,#4938,#4939,#4940,#4941),.UNSPECIFIED.,.F.,.F.)
B_SPLINE_CURVE_WITH_KNOTS((3,2,2,2,2,2,2,2,3),(0.45,0.4525,0.455,0.4575,
0.46,0.4625,0.465,0.4675,0.47),.UNSPECIFIED.)
CURVE()
GEOMETRIC_REPRESENTATION_ITEM()
RATIONAL_B_SPLINE_CURVE((1.,0.923879532511287,1.,0.923879532511287,1.,0.923879532511287,
1.,0.923879532511287,1.,0.923879532511287,1.,0.923879532511287,1.,0.923879532511287,
1.,0.923879532511287,1.))
REPRESENTATION_ITEM('')
);
#625=(
BOUNDED_CURVE()
B_SPLINE_CURVE(2,(#4942,#4943,#4944,#4945,#4946,#4947,#4948,#4949,#4950,
#4951,#4952,#4953,#4954,#4955,#4956,#4957,#4958),.UNSPECIFIED.,.F.,.F.)
B_SPLINE_CURVE_WITH_KNOTS((3,2,2,2,2,2,2,2,3),(0.45,0.4525,0.455,0.4575,
0.46,0.4625,0.465,0.4675,0.47),.UNSPECIFIED.)
CURVE()
GEOMETRIC_REPRESENTATION_ITEM()
RATIONAL_B_SPLINE_CURVE((1.,0.923879532511287,1.,0.923879532511287,1.,0.923879532511287,
1.,0.923879532511287,1.,0.923879532511287,1.,0.923879532511287,1.,0.923879532511287,
1.,0.923879532511287,1.))
REPRESENTATION_ITEM('')
);
#626=(
BOUNDED_CURVE()
B_SPLINE_CURVE(2,(#4963,#4964,#4965,#4966,#4967,#4968,#4969,#4970,#4971,
#4972,#4973,#4974,#4975,#4976,#4977,#4978,#4979),.UNSPECIFIED.,.F.,.F.)
B_SPLINE_CURVE_WITH_KNOTS((3,2,2,2,2,2,2,2,3),(0.43,0.4325,0.435,0.4375,
0.44,0.4425,0.445,0.4475,0.45),.UNSPECIFIED.)
CURVE()
GEOMETRIC_REPRESENTATION_ITEM()
RATIONAL_B_SPLINE_CURVE((1.,0.923879532511287,1.,0.923879532511287,1.,0.923879532511287,
1.,0.923879532511287,1.,0.923879532511287,1.,0.923879532511287,1.,0.923879532511287,
1.,0.923879532511287,1.))
REPRESENTATION_ITEM('')
);
#627=(
BOUNDED_CURVE()
B_SPLINE_CURVE(2,(#4980,#4981,#4982,#4983,#4984,#4985,#4986,#4987,#4988,
#4989,#4990,#4991,#4992,#4993,#4994,#4995,#4996),.UNSPECIFIED.,.F.,.F.)
B_SPLINE_CURVE_WITH_KNOTS((3,2,2,2,2,2,2,2,3),(0.43,0.4325,0.435,0.4375,
0.44,0.4425,0.445,0.4475,0.45),.UNSPECIFIED.)
CURVE()
GEOMETRIC_REPRESENTATION_ITEM()
RATIONAL_B_SPLINE_CURVE((1.,0.923879532511287,1.,0.923879532511287,1.,0.923879532511287,
1.,0.923879532511287,1.,0.923879532511287,1.,0.923879532511287,1.,0.923879532511287,
1.,0.923879532511287,1.))
REPRESENTATION_ITEM('')
);
#628=(
BOUNDED_CURVE()
B_SPLINE_CURVE(2,(#5001,#5002,#5003,#5004,#5005,#5006,#5007,#5008,#5009,
#5010,#5011,#5012,#5013,#5014,#5015,#5016,#5017),.UNSPECIFIED.,.F.,.F.)
B_SPLINE_CURVE_WITH_KNOTS((3,2,2,2,2,2,2,2,3),(0.41,0.4125,0.415,0.4175,
0.42,0.4225,0.425,0.4275,0.43),.UNSPECIFIED.)
CURVE()
GEOMETRIC_REPRESENTATION_ITEM()
RATIONAL_B_SPLINE_CURVE((1.,0.923879532511287,1.,0.923879532511287,1.,0.923879532511287,
1.,0.923879532511287,1.,0.923879532511287,1.,0.923879532511287,1.,0.923879532511287,
1.,0.923879532511287,1.))
REPRESENTATION_ITEM('')
);
#629=(
BOUNDED_CURVE()
B_SPLINE_CURVE(2,(#5018,#5019,#5020,#5021,#5022,#5023,#5024,#5025,#5026,
#5027,#5028,#5029,#5030,#5031,#5032,#5033,#5034),.UNSPECIFIED.,.F.,.F.)
B_SPLINE_CURVE_WITH_KNOTS((3,2,2,2,2,2,2,2,3),(0.41,0.4125,0.415,0.4175,
0.42,0.4225,0.425,0.4275,0.43),.UNSPECIFIED.)
CURVE()
GEOMETRIC_REPRESENTATION_ITEM()
RATIONAL_B_SPLINE_CURVE((1.,0.923879532511287,1.,0.923879532511287,1.,0.923879532511287,
1.,0.923879532511287,1.,0.923879532511287,1.,0.923879532511287,1.,0.923879532511287,
1.,0.923879532511287,1.))
REPRESENTATION_ITEM('')
);
#630=(
BOUNDED_CURVE()
B_SPLINE_CURVE(2,(#5039,#5040,#5041,#5042,#5043,#5044,#5045,#5046,#5047,
#5048,#5049,#5050,#5051,#5052,#5053,#5054,#5055),.UNSPECIFIED.,.F.,.F.)
B_SPLINE_CURVE_WITH_KNOTS((3,2,2,2,2,2,2,2,3),(0.39,0.3925,0.395,0.3975,
0.4,0.4025,0.405,0.4075,0.41),.UNSPECIFIED.)
CURVE()
GEOMETRIC_REPRESENTATION_ITEM()
RATIONAL_B_SPLINE_CURVE((1.,0.923879532511287,1.,0.923879532511287,1.,0.923879532511287,
1.,0.923879532511287,1.,0.923879532511287,1.,0.923879532511287,1.,0.923879532511287,
1.,0.923879532511287,1.))
REPRESENTATION_ITEM('')
);
#631=(
BOUNDED_CURVE()
B_SPLINE_CURVE(2,(#5056,#5057,#5058,#5059,#5060,#5061,#5062,#5063,#5064,
#5065,#5066,#5067,#5068,#5069,#5070,#5071,#5072),.UNSPECIFIED.,.F.,.F.)
B_SPLINE_CURVE_WITH_KNOTS((3,2,2,2,2,2,2,2,3),(0.39,0.3925,0.395,0.3975,
0.4,0.4025,0.405,0.4075,0.41),.UNSPECIFIED.)
CURVE()
GEOMETRIC_REPRESENTATION_ITEM()
RATIONAL_B_SPLINE_CURVE((1.,0.923879532511287,1.,0.923879532511287,1.,0.923879532511287,
1.,0.923879532511287,1.,0.923879532511287,1.,0.923879532511287,1.,0.923879532511287,
1.,0.923879532511287,1.))
REPRESENTATION_ITEM('')
);
#632=(
BOUNDED_CURVE()
B_SPLINE_CURVE(2,(#5077,#5078,#5079,#5080,#5081,#5082,#5083,#5084,#5085,
#5086,#5087,#5088,#5089,#5090,#5091,#5092,#5093),.UNSPECIFIED.,.F.,.F.)
B_SPLINE_CURVE_WITH_KNOTS((3,2,2,2,2,2,2,2,3),(0.37,0.3725,0.375,0.3775,
0.38,0.3825,0.385,0.3875,0.39),.UNSPECIFIED.)
CURVE()
GEOMETRIC_REPRESENTATION_ITEM()
RATIONAL_B_SPLINE_CURVE((1.,0.923879532511287,1.,0.923879532511287,1.,0.923879532511287,
1.,0.923879532511287,1.,0.923879532511287,1.,0.923879532511287,1.,0.923879532511287,
1.,0.923879532511287,1.))
REPRESENTATION_ITEM('')
);
#633=(
BOUNDED_CURVE()
B_SPLINE_CURVE(2,(#5094,#5095,#5096,#5097,#5098,#5099,#5100,#5101,#5102,
#5103,#5104,#5105,#5106,#5107,#5108,#5109,#5110),.UNSPECIFIED.,.F.,.F.)
B_SPLINE_CURVE_WITH_KNOTS((3,2,2,2,2,2,2,2,3),(0.37,0.3725,0.375,0.3775,
0.38,0.3825,0.385,0.3875,0.39),.UNSPECIFIED.)
CURVE()
GEOMETRIC_REPRESENTATION_ITEM()
RATIONAL_B_SPLINE_CURVE((1.,0.923879532511287,1.,0.923879532511287,1.,0.923879532511287,
1.,0.923879532511287,1.,0.923879532511287,1.,0.923879532511287,1.,0.923879532511287,
1.,0.923879532511287,1.))
REPRESENTATION_ITEM('')
);
#634=(
BOUNDED_CURVE()
B_SPLINE_CURVE(2,(#5115,#5116,#5117,#5118,#5119,#5120,#5121,#5122,#5123,
#5124,#5125,#5126,#5127,#5128,#5129,#5130,#5131),.UNSPECIFIED.,.F.,.F.)
B_SPLINE_CURVE_WITH_KNOTS((3,2,2,2,2,2,2,2,3),(0.35,0.3525,0.355,0.3575,
0.36,0.3625,0.365,0.3675,0.37),.UNSPECIFIED.)
CURVE()
GEOMETRIC_REPRESENTATION_ITEM()
RATIONAL_B_SPLINE_CURVE((1.,0.923879532511287,1.,0.923879532511287,1.,0.923879532511287,
1.,0.923879532511287,1.,0.923879532511287,1.,0.923879532511287,1.,0.923879532511287,
1.,0.923879532511287,1.))
REPRESENTATION_ITEM('')
);
#635=(
BOUNDED_CURVE()
B_SPLINE_CURVE(2,(#5132,#5133,#5134,#5135,#5136,#5137,#5138,#5139,#5140,
#5141,#5142,#5143,#5144,#5145,#5146,#5147,#5148),.UNSPECIFIED.,.F.,.F.)
B_SPLINE_CURVE_WITH_KNOTS((3,2,2,2,2,2,2,2,3),(0.35,0.3525,0.355,0.3575,
0.36,0.3625,0.365,0.3675,0.37),.UNSPECIFIED.)
CURVE()
GEOMETRIC_REPRESENTATION_ITEM()
RATIONAL_B_SPLINE_CURVE((1.,0.923879532511287,1.,0.923879532511287,1.,0.923879532511287,
1.,0.923879532511287,1.,0.923879532511287,1.,0.923879532511287,1.,0.923879532511287,
1.,0.923879532511287,1.))
REPRESENTATION_ITEM('')
);
#636=(
BOUNDED_CURVE()
B_SPLINE_CURVE(2,(#5153,#5154,#5155,#5156,#5157,#5158,#5159,#5160,#5161,
#5162,#5163,#5164,#5165,#5166,#5167,#5168,#5169),.UNSPECIFIED.,.F.,.F.)
B_SPLINE_CURVE_WITH_KNOTS((3,2,2,2,2,2,2,2,3),(0.33,0.3325,0.335,0.3375,
0.34,0.3425,0.345,0.3475,0.35),.UNSPECIFIED.)
CURVE()
GEOMETRIC_REPRESENTATION_ITEM()
RATIONAL_B_SPLINE_CURVE((1.,0.923879532511287,1.,0.923879532511287,1.,0.923879532511287,
1.,0.923879532511287,1.,0.923879532511287,1.,0.923879532511287,1.,0.923879532511287,
1.,0.923879532511287,1.))
REPRESENTATION_ITEM('')
);
#637=(
BOUNDED_CURVE()
B_SPLINE_CURVE(2,(#5170,#5171,#5172,#5173,#5174,#5175,#5176,#5177,#5178,
#5179,#5180,#5181,#5182,#5183,#5184,#5185,#5186),.UNSPECIFIED.,.F.,.F.)
B_SPLINE_CURVE_WITH_KNOTS((3,2,2,2,2,2,2,2,3),(0.33,0.3325,0.335,0.3375,
0.34,0.3425,0.345,0.3475,0.35),.UNSPECIFIED.)
CURVE()
GEOMETRIC_REPRESENTATION_ITEM()
RATIONAL_B_SPLINE_CURVE((1.,0.923879532511287,1.,0.923879532511287,1.,0.923879532511287,
1.,0.923879532511287,1.,0.923879532511287,1.,0.923879532511287,1.,0.923879532511287,
1.,0.923879532511287,1.))
REPRESENTATION_ITEM('')
);
#638=(
BOUNDED_CURVE()
B_SPLINE_CURVE(2,(#5191,#5192,#5193,#5194,#5195,#5196,#5197,#5198,#5199,
#5200,#5201,#5202,#5203,#5204,#5205,#5206,#5207),.UNSPECIFIED.,.F.,.F.)
B_SPLINE_CURVE_WITH_KNOTS((3,2,2,2,2,2,2,2,3),(0.31,0.3125,0.315,0.3175,
0.32,0.3225,0.325,0.3275,0.33),.UNSPECIFIED.)
CURVE()
GEOMETRIC_REPRESENTATION_ITEM()
RATIONAL_B_SPLINE_CURVE((1.,0.923879532511287,1.,0.923879532511287,1.,0.923879532511287,
1.,0.923879532511287,1.,0.923879532511287,1.,0.923879532511287,1.,0.923879532511287,
1.,0.923879532511287,1.))
REPRESENTATION_ITEM('')
);
#639=(
BOUNDED_CURVE()
B_SPLINE_CURVE(2,(#5208,#5209,#5210,#5211,#5212,#5213,#5214,#5215,#5216,
#5217,#5218,#5219,#5220,#5221,#5222,#5223,#5224),.UNSPECIFIED.,.F.,.F.)
B_SPLINE_CURVE_WITH_KNOTS((3,2,2,2,2,2,2,2,3),(0.31,0.3125,0.315,0.3175,
0.32,0.3225,0.325,0.3275,0.33),.UNSPECIFIED.)
CURVE()
GEOMETRIC_REPRESENTATION_ITEM()
RATIONAL_B_SPLINE_CURVE((1.,0.923879532511287,1.,0.923879532511287,1.,0.923879532511287,
1.,0.923879532511287,1.,0.923879532511287,1.,0.923879532511287,1.,0.923879532511287,
1.,0.923879532511287,1.))
REPRESENTATION_ITEM('')
);
#640=(
BOUNDED_CURVE()
B_SPLINE_CURVE(2,(#5229,#5230,#5231,#5232,#5233,#5234,#5235,#5236,#5237,
#5238,#5239,#5240,#5241,#5242,#5243,#5244,#5245),.UNSPECIFIED.,.F.,.F.)
B_SPLINE_CURVE_WITH_KNOTS((3,2,2,2,2,2,2,2,3),(0.29,0.2925,0.295,0.2975,
0.3,0.3025,0.305,0.3075,0.31),.UNSPECIFIED.)
CURVE()
GEOMETRIC_REPRESENTATION_ITEM()
RATIONAL_B_SPLINE_CURVE((1.,0.923879532511287,1.,0.923879532511287,1.,0.923879532511287,
1.,0.923879532511287,1.,0.923879532511287,1.,0.923879532511287,1.,0.923879532511287,
1.,0.923879532511287,1.))
REPRESENTATION_ITEM('')
);
#641=(
BOUNDED_CURVE()
B_SPLINE_CURVE(2,(#5246,#5247,#5248,#5249,#5250,#5251,#5252,#5253,#5254,
#5255,#5256,#5257,#5258,#5259,#5260,#5261,#5262),.UNSPECIFIED.,.F.,.F.)
B_SPLINE_CURVE_WITH_KNOTS((3,2,2,2,2,2,2,2,3),(0.29,0.2925,0.295,0.2975,
0.3,0.3025,0.305,0.3075,0.31),.UNSPECIFIED.)
CURVE()
GEOMETRIC_REPRESENTATION_ITEM()
RATIONAL_B_SPLINE_CURVE((1.,0.923879532511287,1.,0.923879532511287,1.,0.923879532511287,
1.,0.923879532511287,1.,0.923879532511287,1.,0.923879532511287,1.,0.923879532511287,
1.,0.923879532511287,1.))
REPRESENTATION_ITEM('')
);
#642=(
BOUNDED_CURVE()
B_SPLINE_CURVE(2,(#5267,#5268,#5269,#5270,#5271,#5272,#5273,#5274,#5275,
#5276,#5277,#5278,#5279,#5280,#5281,#5282,#5283),.UNSPECIFIED.,.F.,.F.)
B_SPLINE_CURVE_WITH_KNOTS((3,2,2,2,2,2,2,2,3),(0.27,0.2725,0.275,0.2775,
0.28,0.2825,0.285,0.2875,0.29),.UNSPECIFIED.)
CURVE()
GEOMETRIC_REPRESENTATION_ITEM()
RATIONAL_B_SPLINE_CURVE((1.,0.923879532511287,1.,0.923879532511287,1.,0.923879532511287,
1.,0.923879532511287,1.,0.923879532511287,1.,0.923879532511287,1.,0.923879532511287,
1.,0.923879532511287,1.))
REPRESENTATION_ITEM('')
);
#643=(
BOUNDED_CURVE()
B_SPLINE_CURVE(2,(#5284,#5285,#5286,#5287,#5288,#5289,#5290,#5291,#5292,
#5293,#5294,#5295,#5296,#5297,#5298,#5299,#5300),.UNSPECIFIED.,.F.,.F.)
B_SPLINE_CURVE_WITH_KNOTS((3,2,2,2,2,2,2,2,3),(0.27,0.2725,0.275,0.2775,
0.28,0.2825,0.285,0.2875,0.29),.UNSPECIFIED.)
CURVE()
GEOMETRIC_REPRESENTATION_ITEM()
RATIONAL_B_SPLINE_CURVE((1.,0.923879532511287,1.,0.923879532511287,1.,0.923879532511287,
1.,0.923879532511287,1.,0.923879532511287,1.,0.923879532511287,1.,0.923879532511287,
1.,0.923879532511287,1.))
REPRESENTATION_ITEM('')
);
#644=(
BOUNDED_CURVE()
B_SPLINE_CURVE(2,(#5305,#5306,#5307,#5308,#5309,#5310,#5311,#5312,#5313,
#5314,#5315,#5316,#5317,#5318,#5319,#5320,#5321),.UNSPECIFIED.,.F.,.F.)
B_SPLINE_CURVE_WITH_KNOTS((3,2,2,2,2,2,2,2,3),(0.25,0.2525,0.255,0.2575,
0.26,0.2625,0.265,0.2675,0.27),.UNSPECIFIED.)
CURVE()
GEOMETRIC_REPRESENTATION_ITEM()
RATIONAL_B_SPLINE_CURVE((1.,0.923879532511287,1.,0.923879532511287,1.,0.923879532511287,
1.,0.923879532511287,1.,0.923879532511287,1.,0.923879532511287,1.,0.923879532511287,
1.,0.923879532511287,1.))
REPRESENTATION_ITEM('')
);
#645=(
BOUNDED_CURVE()
B_SPLINE_CURVE(2,(#5322,#5323,#5324,#5325,#5326,#5327,#5328,#5329,#5330,
#5331,#5332,#5333,#5334,#5335,#5336,#5337,#5338),.UNSPECIFIED.,.F.,.F.)
B_SPLINE_CURVE_WITH_KNOTS((3,2,2,2,2,2,2,2,3),(0.25,0.2525,0.255,0.2575,
0.26,0.2625,0.265,0.2675,0.27),.UNSPECIFIED.)
CURVE()
GEOMETRIC_REPRESENTATION_ITEM()
RATIONAL_B_SPLINE_CURVE((1.,0.923879532511287,1.,0.923879532511287,1.,0.923879532511287,
1.,0.923879532511287,1.,0.923879532511287,1.,0.923879532511287,1.,0.923879532511287,
1.,0.923879532511287,1.))
REPRESENTATION_ITEM('')
);
#646=(
BOUNDED_CURVE()
B_SPLINE_CURVE(2,(#5343,#5344,#5345,#5346,#5347,#5348,#5349,#5350,#5351,
#5352,#5353,#5354,#5355,#5356,#5357,#5358,#5359),.UNSPECIFIED.,.F.,.F.)
B_SPLINE_CURVE_WITH_KNOTS((3,2,2,2,2,2,2,2,3),(0.23,0.2325,0.235,0.2375,
0.24,0.2425,0.245,0.2475,0.25),.UNSPECIFIED.)
CURVE()
GEOMETRIC_REPRESENTATION_ITEM()
RATIONAL_B_SPLINE_CURVE((1.,0.923879532511287,1.,0.923879532511287,1.,0.923879532511287,
1.,0.923879532511287,1.,0.923879532511287,1.,0.923879532511287,1.,0.923879532511287,
1.,0.923879532511287,1.))
REPRESENTATION_ITEM('')
);
#647=(
BOUNDED_CURVE()
B_SPLINE_CURVE(2,(#5360,#5361,#5362,#5363,#5364,#5365,#5366,#5367,#5368,
#5369,#5370,#5371,#5372,#5373,#5374,#5375,#5376),.UNSPECIFIED.,.F.,.F.)
B_SPLINE_CURVE_WITH_KNOTS((3,2,2,2,2,2,2,2,3),(0.23,0.2325,0.235,0.2375,
0.24,0.2425,0.245,0.2475,0.25),.UNSPECIFIED.)
CURVE()
GEOMETRIC_REPRESENTATION_ITEM()
RATIONAL_B_SPLINE_CURVE((1.,0.923879532511287,1.,0.923879532511287,1.,0.923879532511287,
1.,0.923879532511287,1.,0.923879532511287,1.,0.923879532511287,1.,0.923879532511287,
1.,0.923879532511287,1.))
REPRESENTATION_ITEM('')
);
#648=(
BOUNDED_CURVE()
B_SPLINE_CURVE(2,(#5381,#5382,#5383,#5384,#5385,#5386,#5387,#5388,#5389,
#5390,#5391,#5392,#5393,#5394,#5395,#5396,#5397),.UNSPECIFIED.,.F.,.F.)
B_SPLINE_CURVE_WITH_KNOTS((3,2,2,2,2,2,2,2,3),(0.21,0.2125,0.215,0.2175,
0.22,0.2225,0.225,0.2275,0.23),.UNSPECIFIED.)
CURVE()
GEOMETRIC_REPRESENTATION_ITEM()
RATIONAL_B_SPLINE_CURVE((1.,0.923879532511287,1.,0.923879532511287,1.,0.923879532511287,
1.,0.923879532511287,1.,0.923879532511287,1.,0.923879532511287,1.,0.923879532511287,
1.,0.923879532511287,1.))
REPRESENTATION_ITEM('')
);
#649=(
BOUNDED_CURVE()
B_SPLINE_CURVE(2,(#5398,#5399,#5400,#5401,#5402,#5403,#5404,#5405,#5406,
#5407,#5408,#5409,#5410,#5411,#5412,#5413,#5414),.UNSPECIFIED.,.F.,.F.)
B_SPLINE_CURVE_WITH_KNOTS((3,2,2,2,2,2,2,2,3),(0.21,0.2125,0.215,0.2175,
0.22,0.2225,0.225,0.2275,0.23),.UNSPECIFIED.)
CURVE()
GEOMETRIC_REPRESENTATION_ITEM()
RATIONAL_B_SPLINE_CURVE((1.,0.923879532511287,1.,0.923879532511287,1.,0.923879532511287,
1.,0.923879532511287,1.,0.923879532511287,1.,0.923879532511287,1.,0.923879532511287,
1.,0.923879532511287,1.))
REPRESENTATION_ITEM('')
);
#650=(
BOUNDED_CURVE()
B_SPLINE_CURVE(2,(#5419,#5420,#5421,#5422,#5423,#5424,#5425,#5426,#5427,
#5428,#5429,#5430,#5431,#5432,#5433,#5434,#5435),.UNSPECIFIED.,.F.,.F.)
B_SPLINE_CURVE_WITH_KNOTS((3,2,2,2,2,2,2,2,3),(0.19,0.1925,0.195,0.1975,
0.2,0.2025,0.205,0.2075,0.21),.UNSPECIFIED.)
CURVE()
GEOMETRIC_REPRESENTATION_ITEM()
RATIONAL_B_SPLINE_CURVE((1.,0.923879532511287,1.,0.923879532511287,1.,0.923879532511287,
1.,0.923879532511287,1.,0.923879532511287,1.,0.923879532511287,1.,0.923879532511287,
1.,0.923879532511287,1.))
REPRESENTATION_ITEM('')
);
#651=(
BOUNDED_CURVE()
B_SPLINE_CURVE(2,(#5436,#5437,#5438,#5439,#5440,#5441,#5442,#5443,#5444,
#5445,#5446,#5447,#5448,#5449,#5450,#5451,#5452),.UNSPECIFIED.,.F.,.F.)
B_SPLINE_CURVE_WITH_KNOTS((3,2,2,2,2,2,2,2,3),(0.19,0.1925,0.195,0.1975,
0.2,0.2025,0.205,0.2075,0.21),.UNSPECIFIED.)
CURVE()
GEOMETRIC_REPRESENTATION_ITEM()
RATIONAL_B_SPLINE_CURVE((1.,0.923879532511287,1.,0.923879532511287,1.,0.923879532511287,
1.,0.923879532511287,1.,0.923879532511287,1.,0.923879532511287,1.,0.923879532511287,
1.,0.923879532511287,1.))
REPRESENTATION_ITEM('')
);
#652=(
BOUNDED_CURVE()
B_SPLINE_CURVE(2,(#5457,#5458,#5459,#5460,#5461,#5462,#5463,#5464,#5465,
#5466,#5467,#5468,#5469,#5470,#5471,#5472,#5473),.UNSPECIFIED.,.F.,.F.)
B_SPLINE_CURVE_WITH_KNOTS((3,2,2,2,2,2,2,2,3),(0.17,0.1725,0.175,0.1775,
0.18,0.1825,0.185,0.1875,0.19),.UNSPECIFIED.)
CURVE()
GEOMETRIC_REPRESENTATION_ITEM()
RATIONAL_B_SPLINE_CURVE((1.,0.923879532511287,1.,0.923879532511287,1.,0.923879532511287,
1.,0.923879532511287,1.,0.923879532511287,1.,0.923879532511287,1.,0.923879532511287,
1.,0.923879532511287,1.))
REPRESENTATION_ITEM('')
);
#653=(
BOUNDED_CURVE()
B_SPLINE_CURVE(2,(#5474,#5475,#5476,#5477,#5478,#5479,#5480,#5481,#5482,
#5483,#5484,#5485,#5486,#5487,#5488,#5489,#5490),.UNSPECIFIED.,.F.,.F.)
B_SPLINE_CURVE_WITH_KNOTS((3,2,2,2,2,2,2,2,3),(0.17,0.1725,0.175,0.1775,
0.18,0.1825,0.185,0.1875,0.19),.UNSPECIFIED.)
CURVE()
GEOMETRIC_REPRESENTATION_ITEM()
RATIONAL_B_SPLINE_CURVE((1.,0.923879532511287,1.,0.923879532511287,1.,0.923879532511287,
1.,0.923879532511287,1.,0.923879532511287,1.,0.923879532511287,1.,0.923879532511287,
1.,0.923879532511287,1.))
REPRESENTATION_ITEM('')
);
#654=(
BOUNDED_CURVE()
B_SPLINE_CURVE(2,(#5495,#5496,#5497,#5498,#5499,#5500,#5501,#5502,#5503,
#5504,#5505,#5506,#5507,#5508,#5509,#5510,#5511),.UNSPECIFIED.,.F.,.F.)
B_SPLINE_CURVE_WITH_KNOTS((3,2,2,2,2,2,2,2,3),(0.15,0.1525,0.155,0.1575,
0.16,0.1625,0.165,0.1675,0.17),.UNSPECIFIED.)
CURVE()
GEOMETRIC_REPRESENTATION_ITEM()
RATIONAL_B_SPLINE_CURVE((1.,0.923879532511287,1.,0.923879532511287,1.,0.923879532511287,
1.,0.923879532511287,1.,0.923879532511287,1.,0.923879532511287,1.,0.923879532511287,
1.,0.923879532511287,1.))
REPRESENTATION_ITEM('')
);
#655=(
BOUNDED_CURVE()
B_SPLINE_CURVE(2,(#5512,#5513,#5514,#5515,#5516,#5517,#5518,#5519,#5520,
#5521,#5522,#5523,#5524,#5525,#5526,#5527,#5528),.UNSPECIFIED.,.F.,.F.)
B_SPLINE_CURVE_WITH_KNOTS((3,2,2,2,2,2,2,2,3),(0.15,0.1525,0.155,0.1575,
0.16,0.1625,0.165,0.1675,0.17),.UNSPECIFIED.)
CURVE()
GEOMETRIC_REPRESENTATION_ITEM()
RATIONAL_B_SPLINE_CURVE((1.,0.923879532511287,1.,0.923879532511287,1.,0.923879532511287,
1.,0.923879532511287,1.,0.923879532511287,1.,0.923879532511287,1.,0.923879532511287,
1.,0.923879532511287,1.))
REPRESENTATION_ITEM('')
);
#656=(
BOUNDED_CURVE()
B_SPLINE_CURVE(2,(#5533,#5534,#5535,#5536,#5537,#5538,#5539,#5540,#5541,
#5542,#5543,#5544,#5545,#5546,#5547,#5548,#5549),.UNSPECIFIED.,.F.,.F.)
B_SPLINE_CURVE_WITH_KNOTS((3,2,2,2,2,2,2,2,3),(0.13,0.1325,0.135,0.1375,
0.14,0.1425,0.145,0.1475,0.15),.UNSPECIFIED.)
CURVE()
GEOMETRIC_REPRESENTATION_ITEM()
RATIONAL_B_SPLINE_CURVE((1.,0.923879532511287,1.,0.923879532511287,1.,0.923879532511287,
1.,0.923879532511287,1.,0.923879532511287,1.,0.923879532511287,1.,0.923879532511287,
1.,0.923879532511287,1.))
REPRESENTATION_ITEM('')
);
#657=(
BOUNDED_CURVE()
B_SPLINE_CURVE(2,(#5550,#5551,#5552,#5553,#5554,#5555,#5556,#5557,#5558,
#5559,#5560,#5561,#5562,#5563,#5564,#5565,#5566),.UNSPECIFIED.,.F.,.F.)
B_SPLINE_CURVE_WITH_KNOTS((3,2,2,2,2,2,2,2,3),(0.13,0.1325,0.135,0.1375,
0.14,0.1425,0.145,0.1475,0.15),.UNSPECIFIED.)
CURVE()
GEOMETRIC_REPRESENTATION_ITEM()
RATIONAL_B_SPLINE_CURVE((1.,0.923879532511287,1.,0.923879532511287,1.,0.923879532511287,
1.,0.923879532511287,1.,0.923879532511287,1.,0.923879532511287,1.,0.923879532511287,
1.,0.923879532511287,1.))
REPRESENTATION_ITEM('')
);
#658=(
BOUNDED_CURVE()
B_SPLINE_CURVE(2,(#5571,#5572,#5573,#5574,#5575,#5576,#5577,#5578,#5579,
#5580,#5581,#5582,#5583,#5584,#5585,#5586,#5587),.UNSPECIFIED.,.F.,.F.)
B_SPLINE_CURVE_WITH_KNOTS((3,2,2,2,2,2,2,2,3),(0.11,0.1125,0.115,0.1175,
0.12,0.1225,0.125,0.1275,0.13),.UNSPECIFIED.)
CURVE()
GEOMETRIC_REPRESENTATION_ITEM()
RATIONAL_B_SPLINE_CURVE((1.,0.923879532511287,1.,0.923879532511287,1.,0.923879532511287,
1.,0.923879532511287,1.,0.923879532511287,1.,0.923879532511287,1.,0.923879532511287,
1.,0.923879532511287,1.))
REPRESENTATION_ITEM('')
);
#659=(
BOUNDED_CURVE()
B_SPLINE_CURVE(2,(#5588,#5589,#5590,#5591,#5592,#5593,#5594,#5595,#5596,
#5597,#5598,#5599,#5600,#5601,#5602,#5603,#5604),.UNSPECIFIED.,.F.,.F.)
B_SPLINE_CURVE_WITH_KNOTS((3,2,2,2,2,2,2,2,3),(0.11,0.1125,0.115,0.1175,
0.12,0.1225,0.125,0.1275,0.13),.UNSPECIFIED.)
CURVE()
GEOMETRIC_REPRESENTATION_ITEM()
RATIONAL_B_SPLINE_CURVE((1.,0.923879532511287,1.,0.923879532511287,1.,0.923879532511287,
1.,0.923879532511287,1.,0.923879532511287,1.,0.923879532511287,1.,0.923879532511287,
1.,0.923879532511287,1.))
REPRESENTATION_ITEM('')
);
#660=(
BOUNDED_CURVE()
B_SPLINE_CURVE(2,(#5609,#5610,#5611,#5612,#5613,#5614,#5615,#5616,#5617,
#5618,#5619,#5620,#5621,#5622,#5623,#5624,#5625),.UNSPECIFIED.,.F.,.F.)
B_SPLINE_CURVE_WITH_KNOTS((3,2,2,2,2,2,2,2,3),(0.09,0.0925,0.095,0.0975,
0.1,0.1025,0.105,0.1075,0.11),.UNSPECIFIED.)
CURVE()
GEOMETRIC_REPRESENTATION_ITEM()
RATIONAL_B_SPLINE_CURVE((1.,0.923879532511287,1.,0.923879532511287,1.,0.923879532511287,
1.,0.923879532511287,1.,0.923879532511287,1.,0.923879532511287,1.,0.923879532511287,
1.,0.923879532511287,1.))
REPRESENTATION_ITEM('')
);
#661=(
BOUNDED_CURVE()
B_SPLINE_CURVE(2,(#5626,#5627,#5628,#5629,#5630,#5631,#5632,#5633,#5634,
#5635,#5636,#5637,#5638,#5639,#5640,#5641,#5642),.UNSPECIFIED.,.F.,.F.)
B_SPLINE_CURVE_WITH_KNOTS((3,2,2,2,2,2,2,2,3),(0.09,0.0925,0.095,0.0975,
0.1,0.1025,0.105,0.1075,0.11),.UNSPECIFIED.)
CURVE()
GEOMETRIC_REPRESENTATION_ITEM()
RATIONAL_B_SPLINE_CURVE((1.,0.923879532511287,1.,0.923879532511287,1.,0.923879532511287,
1.,0.923879532511287,1.,0.923879532511287,1.,0.923879532511287,1.,0.923879532511287,
1.,0.923879532511287,1.))
REPRESENTATION_ITEM('')
);
#662=(
BOUNDED_CURVE()
B_SPLINE_CURVE(2,(#5647,#5648,#5649,#5650,#5651,#5652,#5653,#5654,#5655,
#5656,#5657,#5658,#5659,#5660,#5661,#5662,#5663),.UNSPECIFIED.,.F.,.F.)
B_SPLINE_CURVE_WITH_KNOTS((3,2,2,2,2,2,2,2,3),(0.07,0.0725,0.075,0.0775,
0.08,0.0825,0.085,0.0875,0.09),.UNSPECIFIED.)
CURVE()
GEOMETRIC_REPRESENTATION_ITEM()
RATIONAL_B_SPLINE_CURVE((1.,0.923879532511287,1.,0.923879532511287,1.,0.923879532511287,
1.,0.923879532511287,1.,0.923879532511287,1.,0.923879532511287,1.,0.923879532511287,
1.,0.923879532511287,1.))
REPRESENTATION_ITEM('')
);
#663=(
BOUNDED_CURVE()
B_SPLINE_CURVE(2,(#5664,#5665,#5666,#5667,#5668,#5669,#5670,#5671,#5672,
#5673,#5674,#5675,#5676,#5677,#5678,#5679,#5680),.UNSPECIFIED.,.F.,.F.)
B_SPLINE_CURVE_WITH_KNOTS((3,2,2,2,2,2,2,2,3),(0.07,0.0725,0.075,0.0775,
0.08,0.0825,0.085,0.0875,0.09),.UNSPECIFIED.)
CURVE()
GEOMETRIC_REPRESENTATION_ITEM()
RATIONAL_B_SPLINE_CURVE((1.,0.923879532511287,1.,0.923879532511287,1.,0.923879532511287,
1.,0.923879532511287,1.,0.923879532511287,1.,0.923879532511287,1.,0.923879532511287,
1.,0.923879532511287,1.))
REPRESENTATION_ITEM('')
);
#664=(
BOUNDED_CURVE()
B_SPLINE_CURVE(2,(#5685,#5686,#5687,#5688,#5689,#5690,#5691,#5692,#5693,
#5694,#5695,#5696,#5697,#5698,#5699,#5700,#5701),.UNSPECIFIED.,.F.,.F.)
B_SPLINE_CURVE_WITH_KNOTS((3,2,2,2,2,2,2,2,3),(0.05,0.0525,0.055,0.0575,
0.06,0.0625,0.065,0.0675,0.07),.UNSPECIFIED.)
CURVE()
GEOMETRIC_REPRESENTATION_ITEM()
RATIONAL_B_SPLINE_CURVE((1.,0.923879532511287,1.,0.923879532511287,1.,0.923879532511287,
1.,0.923879532511287,1.,0.923879532511287,1.,0.923879532511287,1.,0.923879532511287,
1.,0.923879532511287,1.))
REPRESENTATION_ITEM('')
);
#665=(
BOUNDED_CURVE()
B_SPLINE_CURVE(2,(#5702,#5703,#5704,#5705,#5706,#5707,#5708,#5709,#5710,
#5711,#5712,#5713,#5714,#5715,#5716,#5717,#5718),.UNSPECIFIED.,.F.,.F.)
B_SPLINE_CURVE_WITH_KNOTS((3,2,2,2,2,2,2,2,3),(0.05,0.0525,0.055,0.0575,
0.06,0.0625,0.065,0.0675,0.07),.UNSPECIFIED.)
CURVE()
GEOMETRIC_REPRESENTATION_ITEM()
RATIONAL_B_SPLINE_CURVE((1.,0.923879532511287,1.,0.923879532511287,1.,0.923879532511287,
1.,0.923879532511287,1.,0.923879532511287,1.,0.923879532511287,1.,0.923879532511287,
1.,0.923879532511287,1.))
REPRESENTATION_ITEM('')
);
#666=(
BOUNDED_CURVE()
B_SPLINE_CURVE(2,(#5723,#5724,#5725,#5726,#5727,#5728,#5729,#5730,#5731,
#5732,#5733,#5734,#5735,#5736,#5737,#5738,#5739),.UNSPECIFIED.,.F.,.F.)
B_SPLINE_CURVE_WITH_KNOTS((3,2,2,2,2,2,2,2,3),(0.03,0.0325,0.035,0.0375,
0.04,0.0425,0.045,0.0475,0.05),.UNSPECIFIED.)
CURVE()
GEOMETRIC_REPRESENTATION_ITEM()
RATIONAL_B_SPLINE_CURVE((1.,0.923879532511287,1.,0.923879532511287,1.,0.923879532511287,
1.,0.923879532511287,1.,0.923879532511287,1.,0.923879532511287,1.,0.923879532511287,
1.,0.923879532511287,1.))
REPRESENTATION_ITEM('')
);
#667=(
BOUNDED_CURVE()
B_SPLINE_CURVE(2,(#5740,#5741,#5742,#5743,#5744,#5745,#5746,#5747,#5748,
#5749,#5750,#5751,#5752,#5753,#5754,#5755,#5756),.UNSPECIFIED.,.F.,.F.)
B_SPLINE_CURVE_WITH_KNOTS((3,2,2,2,2,2,2,2,3),(0.03,0.0325,0.035,0.0375,
0.04,0.0425,0.045,0.0475,0.05),.UNSPECIFIED.)
CURVE()
GEOMETRIC_REPRESENTATION_ITEM()
RATIONAL_B_SPLINE_CURVE((1.,0.923879532511287,1.,0.923879532511287,1.,0.923879532511287,
1.,0.923879532511287,1.,0.923879532511287,1.,0.923879532511287,1.,0.923879532511287,
1.,0.923879532511287,1.))
REPRESENTATION_ITEM('')
);
#668=(
BOUNDED_CURVE()
B_SPLINE_CURVE(2,(#5762,#5763,#5764,#5765,#5766,#5767,#5768,#5769,#5770),
 .UNSPECIFIED.,.F.,.F.)
B_SPLINE_CURVE_WITH_KNOTS((3,2,2,2,3),(0.,0.0025,0.005,0.0075,0.01),
 .UNSPECIFIED.)
CURVE()
GEOMETRIC_REPRESENTATION_ITEM()
RATIONAL_B_SPLINE_CURVE((1.,0.923879532511287,1.,0.923879532511287,1.,0.923879532511287,
1.,0.923879532511287,1.))
REPRESENTATION_ITEM('')
);
#669=(
BOUNDED_CURVE()
B_SPLINE_CURVE(2,(#5773,#5774,#5775,#5776,#5777,#5778,#5779,#5780,#5781),
 .UNSPECIFIED.,.F.,.F.)
B_SPLINE_CURVE_WITH_KNOTS((3,2,2,2,3),(0.,0.0025,0.005,0.0075,0.01),
 .UNSPECIFIED.)
CURVE()
GEOMETRIC_REPRESENTATION_ITEM()
RATIONAL_B_SPLINE_CURVE((1.,0.923879532511287,1.,0.923879532511287,1.,0.923879532511287,
1.,0.923879532511287,1.))
REPRESENTATION_ITEM('')
);
#670=(
BOUNDED_CURVE()
B_SPLINE_CURVE(2,(#5787,#5788,#5789,#5790,#5791),.UNSPECIFIED.,.F.,.F.)
B_SPLINE_CURVE_WITH_KNOTS((3,2,3),(0.995,0.9975,1.),.UNSPECIFIED.)
CURVE()
GEOMETRIC_REPRESENTATION_ITEM()
RATIONAL_B_SPLINE_CURVE((1.,0.923879532511287,1.,0.923879532511287,1.))
REPRESENTATION_ITEM('')
);
#671=(
BOUNDED_CURVE()
B_SPLINE_CURVE(2,(#5794,#5795,#5796,#5797,#5798,#5799,#5800),
 .UNSPECIFIED.,.F.,.F.)
B_SPLINE_CURVE_WITH_KNOTS((3,2,2,3),(0.975,0.9775,0.98,0.9825),
 .UNSPECIFIED.)
CURVE()
GEOMETRIC_REPRESENTATION_ITEM()
RATIONAL_B_SPLINE_CURVE((1.,0.923879532511287,1.,0.923879532511287,1.,0.923879532511287,
1.))
REPRESENTATION_ITEM('')
);
#672=(
BOUNDED_CURVE()
B_SPLINE_CURVE(2,(#5805,#5806,#5807,#5808,#5809,#5810,#5811,#5812,#5813,
#5814,#5815,#5816,#5817,#5818,#5819,#5820,#5821),.UNSPECIFIED.,.F.,.F.)
B_SPLINE_CURVE_WITH_KNOTS((3,2,2,2,2,2,2,2,3),(0.975,0.9775,0.98,0.9825,
0.985,0.9875,0.99,0.9925,0.995),.UNSPECIFIED.)
CURVE()
GEOMETRIC_REPRESENTATION_ITEM()
RATIONAL_B_SPLINE_CURVE((1.,0.923879532511287,1.,0.923879532511287,1.,0.923879532511287,
1.,0.923879532511287,1.,0.923879532511287,1.,0.923879532511287,1.,0.923879532511287,
1.,0.923879532511287,1.))
REPRESENTATION_ITEM('')
);
#673=(
BOUNDED_CURVE()
B_SPLINE_CURVE(2,(#5822,#5823,#5824,#5825,#5826,#5827,#5828,#5829,#5830,
#5831,#5832,#5833,#5834,#5835,#5836,#5837,#5838),.UNSPECIFIED.,.F.,.F.)
B_SPLINE_CURVE_WITH_KNOTS((3,2,2,2,2,2,2,2,3),(0.955,0.9575,0.96,0.9625,
0.965,0.9675,0.97,0.9725,0.975),.UNSPECIFIED.)
CURVE()
GEOMETRIC_REPRESENTATION_ITEM()
RATIONAL_B_SPLINE_CURVE((1.,0.923879532511287,1.,0.923879532511287,1.,0.923879532511287,
1.,0.923879532511287,1.,0.923879532511287,1.,0.923879532511287,1.,0.923879532511287,
1.,0.923879532511287,1.))
REPRESENTATION_ITEM('')
);
#674=(
BOUNDED_CURVE()
B_SPLINE_CURVE(2,(#5843,#5844,#5845,#5846,#5847,#5848,#5849,#5850,#5851,
#5852,#5853,#5854,#5855,#5856,#5857,#5858,#5859),.UNSPECIFIED.,.F.,.F.)
B_SPLINE_CURVE_WITH_KNOTS((3,2,2,2,2,2,2,2,3),(0.955,0.9575,0.96,0.9625,
0.965,0.9675,0.97,0.9725,0.975),.UNSPECIFIED.)
CURVE()
GEOMETRIC_REPRESENTATION_ITEM()
RATIONAL_B_SPLINE_CURVE((1.,0.923879532511287,1.,0.923879532511287,1.,0.923879532511287,
1.,0.923879532511287,1.,0.923879532511287,1.,0.923879532511287,1.,0.923879532511287,
1.,0.923879532511287,1.))
REPRESENTATION_ITEM('')
);
#675=(
BOUNDED_CURVE()
B_SPLINE_CURVE(2,(#5860,#5861,#5862,#5863,#5864,#5865,#5866,#5867,#5868,
#5869,#5870,#5871,#5872,#5873,#5874,#5875,#5876),.UNSPECIFIED.,.F.,.F.)
B_SPLINE_CURVE_WITH_KNOTS((3,2,2,2,2,2,2,2,3),(0.935,0.9375,0.94,0.9425,
0.945,0.9475,0.95,0.9525,0.955),.UNSPECIFIED.)
CURVE()
GEOMETRIC_REPRESENTATION_ITEM()
RATIONAL_B_SPLINE_CURVE((1.,0.923879532511287,1.,0.923879532511287,1.,0.923879532511287,
1.,0.923879532511287,1.,0.923879532511287,1.,0.923879532511287,1.,0.923879532511287,
1.,0.923879532511287,1.))
REPRESENTATION_ITEM('')
);
#676=(
BOUNDED_CURVE()
B_SPLINE_CURVE(2,(#5881,#5882,#5883,#5884,#5885,#5886,#5887,#5888,#5889,
#5890,#5891,#5892,#5893,#5894,#5895,#5896,#5897),.UNSPECIFIED.,.F.,.F.)
B_SPLINE_CURVE_WITH_KNOTS((3,2,2,2,2,2,2,2,3),(0.935,0.9375,0.94,0.9425,
0.945,0.9475,0.95,0.9525,0.955),.UNSPECIFIED.)
CURVE()
GEOMETRIC_REPRESENTATION_ITEM()
RATIONAL_B_SPLINE_CURVE((1.,0.923879532511287,1.,0.923879532511287,1.,0.923879532511287,
1.,0.923879532511287,1.,0.923879532511287,1.,0.923879532511287,1.,0.923879532511287,
1.,0.923879532511287,1.))
REPRESENTATION_ITEM('')
);
#677=(
BOUNDED_CURVE()
B_SPLINE_CURVE(2,(#5898,#5899,#5900,#5901,#5902,#5903,#5904,#5905,#5906,
#5907,#5908,#5909,#5910,#5911,#5912,#5913,#5914),.UNSPECIFIED.,.F.,.F.)
B_SPLINE_CURVE_WITH_KNOTS((3,2,2,2,2,2,2,2,3),(0.915,0.9175,0.92,0.9225,
0.925,0.9275,0.93,0.9325,0.935),.UNSPECIFIED.)
CURVE()
GEOMETRIC_REPRESENTATION_ITEM()
RATIONAL_B_SPLINE_CURVE((1.,0.923879532511287,1.,0.923879532511287,1.,0.923879532511287,
1.,0.923879532511287,1.,0.923879532511287,1.,0.923879532511287,1.,0.923879532511287,
1.,0.923879532511287,1.))
REPRESENTATION_ITEM('')
);
#678=(
BOUNDED_CURVE()
B_SPLINE_CURVE(2,(#5919,#5920,#5921,#5922,#5923,#5924,#5925,#5926,#5927,
#5928,#5929,#5930,#5931,#5932,#5933,#5934,#5935),.UNSPECIFIED.,.F.,.F.)
B_SPLINE_CURVE_WITH_KNOTS((3,2,2,2,2,2,2,2,3),(0.915,0.9175,0.92,0.9225,
0.925,0.9275,0.93,0.9325,0.935),.UNSPECIFIED.)
CURVE()
GEOMETRIC_REPRESENTATION_ITEM()
RATIONAL_B_SPLINE_CURVE((1.,0.923879532511287,1.,0.923879532511287,1.,0.923879532511287,
1.,0.923879532511287,1.,0.923879532511287,1.,0.923879532511287,1.,0.923879532511287,
1.,0.923879532511287,1.))
REPRESENTATION_ITEM('')
);
#679=(
BOUNDED_CURVE()
B_SPLINE_CURVE(2,(#5936,#5937,#5938,#5939,#5940,#5941,#5942,#5943,#5944,
#5945,#5946,#5947,#5948,#5949,#5950,#5951,#5952),.UNSPECIFIED.,.F.,.F.)
B_SPLINE_CURVE_WITH_KNOTS((3,2,2,2,2,2,2,2,3),(0.895,0.8975,0.9,0.9025,
0.905,0.9075,0.91,0.9125,0.915),.UNSPECIFIED.)
CURVE()
GEOMETRIC_REPRESENTATION_ITEM()
RATIONAL_B_SPLINE_CURVE((1.,0.923879532511287,1.,0.923879532511287,1.,0.923879532511287,
1.,0.923879532511287,1.,0.923879532511287,1.,0.923879532511287,1.,0.923879532511287,
1.,0.923879532511287,1.))
REPRESENTATION_ITEM('')
);
#680=(
BOUNDED_CURVE()
B_SPLINE_CURVE(2,(#5957,#5958,#5959,#5960,#5961,#5962,#5963,#5964,#5965,
#5966,#5967,#5968,#5969,#5970,#5971,#5972,#5973),.UNSPECIFIED.,.F.,.F.)
B_SPLINE_CURVE_WITH_KNOTS((3,2,2,2,2,2,2,2,3),(0.895,0.8975,0.9,0.9025,
0.905,0.9075,0.91,0.9125,0.915),.UNSPECIFIED.)
CURVE()
GEOMETRIC_REPRESENTATION_ITEM()
RATIONAL_B_SPLINE_CURVE((1.,0.923879532511287,1.,0.923879532511287,1.,0.923879532511287,
1.,0.923879532511287,1.,0.923879532511287,1.,0.923879532511287,1.,0.923879532511287,
1.,0.923879532511287,1.))
REPRESENTATION_ITEM('')
);
#681=(
BOUNDED_CURVE()
B_SPLINE_CURVE(2,(#5974,#5975,#5976,#5977,#5978,#5979,#5980,#5981,#5982,
#5983,#5984,#5985,#5986,#5987,#5988,#5989,#5990),.UNSPECIFIED.,.F.,.F.)
B_SPLINE_CURVE_WITH_KNOTS((3,2,2,2,2,2,2,2,3),(0.875,0.8775,0.88,0.8825,
0.885,0.8875,0.89,0.8925,0.895),.UNSPECIFIED.)
CURVE()
GEOMETRIC_REPRESENTATION_ITEM()
RATIONAL_B_SPLINE_CURVE((1.,0.923879532511287,1.,0.923879532511287,1.,0.923879532511287,
1.,0.923879532511287,1.,0.923879532511287,1.,0.923879532511287,1.,0.923879532511287,
1.,0.923879532511287,1.))
REPRESENTATION_ITEM('')
);
#682=(
BOUNDED_CURVE()
B_SPLINE_CURVE(2,(#5995,#5996,#5997,#5998,#5999,#6000,#6001,#6002,#6003,
#6004,#6005,#6006,#6007,#6008,#6009,#6010,#6011),.UNSPECIFIED.,.F.,.F.)
B_SPLINE_CURVE_WITH_KNOTS((3,2,2,2,2,2,2,2,3),(0.875,0.8775,0.88,0.8825,
0.885,0.8875,0.89,0.8925,0.895),.UNSPECIFIED.)
CURVE()
GEOMETRIC_REPRESENTATION_ITEM()
RATIONAL_B_SPLINE_CURVE((1.,0.923879532511287,1.,0.923879532511287,1.,0.923879532511287,
1.,0.923879532511287,1.,0.923879532511287,1.,0.923879532511287,1.,0.923879532511287,
1.,0.923879532511287,1.))
REPRESENTATION_ITEM('')
);
#683=(
BOUNDED_CURVE()
B_SPLINE_CURVE(2,(#6012,#6013,#6014,#6015,#6016,#6017,#6018,#6019,#6020,
#6021,#6022,#6023,#6024,#6025,#6026,#6027,#6028),.UNSPECIFIED.,.F.,.F.)
B_SPLINE_CURVE_WITH_KNOTS((3,2,2,2,2,2,2,2,3),(0.855,0.8575,0.86,0.8625,
0.865,0.8675,0.87,0.8725,0.875),.UNSPECIFIED.)
CURVE()
GEOMETRIC_REPRESENTATION_ITEM()
RATIONAL_B_SPLINE_CURVE((1.,0.923879532511287,1.,0.923879532511287,1.,0.923879532511287,
1.,0.923879532511287,1.,0.923879532511287,1.,0.923879532511287,1.,0.923879532511287,
1.,0.923879532511287,1.))
REPRESENTATION_ITEM('')
);
#684=(
BOUNDED_CURVE()
B_SPLINE_CURVE(2,(#6033,#6034,#6035,#6036,#6037,#6038,#6039,#6040,#6041,
#6042,#6043,#6044,#6045,#6046,#6047,#6048,#6049),.UNSPECIFIED.,.F.,.F.)
B_SPLINE_CURVE_WITH_KNOTS((3,2,2,2,2,2,2,2,3),(0.855,0.8575,0.86,0.8625,
0.865,0.8675,0.87,0.8725,0.875),.UNSPECIFIED.)
CURVE()
GEOMETRIC_REPRESENTATION_ITEM()
RATIONAL_B_SPLINE_CURVE((1.,0.923879532511287,1.,0.923879532511287,1.,0.923879532511287,
1.,0.923879532511287,1.,0.923879532511287,1.,0.923879532511287,1.,0.923879532511287,
1.,0.923879532511287,1.))
REPRESENTATION_ITEM('')
);
#685=(
BOUNDED_CURVE()
B_SPLINE_CURVE(2,(#6050,#6051,#6052,#6053,#6054,#6055,#6056,#6057,#6058,
#6059,#6060,#6061,#6062,#6063,#6064,#6065,#6066),.UNSPECIFIED.,.F.,.F.)
B_SPLINE_CURVE_WITH_KNOTS((3,2,2,2,2,2,2,2,3),(0.835,0.8375,0.84,0.8425,
0.845,0.8475,0.85,0.8525,0.855),.UNSPECIFIED.)
CURVE()
GEOMETRIC_REPRESENTATION_ITEM()
RATIONAL_B_SPLINE_CURVE((1.,0.923879532511287,1.,0.923879532511287,1.,0.923879532511287,
1.,0.923879532511287,1.,0.923879532511287,1.,0.923879532511287,1.,0.923879532511287,
1.,0.923879532511287,1.))
REPRESENTATION_ITEM('')
);
#686=(
BOUNDED_CURVE()
B_SPLINE_CURVE(2,(#6071,#6072,#6073,#6074,#6075,#6076,#6077,#6078,#6079,
#6080,#6081,#6082,#6083,#6084,#6085,#6086,#6087),.UNSPECIFIED.,.F.,.F.)
B_SPLINE_CURVE_WITH_KNOTS((3,2,2,2,2,2,2,2,3),(0.835,0.8375,0.84,0.8425,
0.845,0.8475,0.85,0.8525,0.855),.UNSPECIFIED.)
CURVE()
GEOMETRIC_REPRESENTATION_ITEM()
RATIONAL_B_SPLINE_CURVE((1.,0.923879532511287,1.,0.923879532511287,1.,0.923879532511287,
1.,0.923879532511287,1.,0.923879532511287,1.,0.923879532511287,1.,0.923879532511287,
1.,0.923879532511287,1.))
REPRESENTATION_ITEM('')
);
#687=(
BOUNDED_CURVE()
B_SPLINE_CURVE(2,(#6088,#6089,#6090,#6091,#6092,#6093,#6094,#6095,#6096,
#6097,#6098,#6099,#6100,#6101,#6102,#6103,#6104),.UNSPECIFIED.,.F.,.F.)
B_SPLINE_CURVE_WITH_KNOTS((3,2,2,2,2,2,2,2,3),(0.815,0.8175,0.82,0.8225,
0.825,0.8275,0.83,0.8325,0.835),.UNSPECIFIED.)
CURVE()
GEOMETRIC_REPRESENTATION_ITEM()
RATIONAL_B_SPLINE_CURVE((1.,0.923879532511287,1.,0.923879532511287,1.,0.923879532511287,
1.,0.923879532511287,1.,0.923879532511287,1.,0.923879532511287,1.,0.923879532511287,
1.,0.923879532511287,1.))
REPRESENTATION_ITEM('')
);
#688=(
BOUNDED_CURVE()
B_SPLINE_CURVE(2,(#6109,#6110,#6111,#6112,#6113,#6114,#6115,#6116,#6117,
#6118,#6119,#6120,#6121,#6122,#6123,#6124,#6125),.UNSPECIFIED.,.F.,.F.)
B_SPLINE_CURVE_WITH_KNOTS((3,2,2,2,2,2,2,2,3),(0.815,0.8175,0.82,0.8225,
0.825,0.8275,0.83,0.8325,0.835),.UNSPECIFIED.)
CURVE()
GEOMETRIC_REPRESENTATION_ITEM()
RATIONAL_B_SPLINE_CURVE((1.,0.923879532511287,1.,0.923879532511287,1.,0.923879532511287,
1.,0.923879532511287,1.,0.923879532511287,1.,0.923879532511287,1.,0.923879532511287,
1.,0.923879532511287,1.))
REPRESENTATION_ITEM('')
);
#689=(
BOUNDED_CURVE()
B_SPLINE_CURVE(2,(#6126,#6127,#6128,#6129,#6130,#6131,#6132,#6133,#6134,
#6135,#6136,#6137,#6138,#6139,#6140,#6141,#6142),.UNSPECIFIED.,.F.,.F.)
B_SPLINE_CURVE_WITH_KNOTS((3,2,2,2,2,2,2,2,3),(0.795,0.7975,0.8,0.8025,
0.805,0.8075,0.81,0.8125,0.815),.UNSPECIFIED.)
CURVE()
GEOMETRIC_REPRESENTATION_ITEM()
RATIONAL_B_SPLINE_CURVE((1.,0.923879532511287,1.,0.923879532511287,1.,0.923879532511287,
1.,0.923879532511287,1.,0.923879532511287,1.,0.923879532511287,1.,0.923879532511287,
1.,0.923879532511287,1.))
REPRESENTATION_ITEM('')
);
#690=(
BOUNDED_CURVE()
B_SPLINE_CURVE(2,(#6147,#6148,#6149,#6150,#6151,#6152,#6153,#6154,#6155,
#6156,#6157,#6158,#6159,#6160,#6161,#6162,#6163),.UNSPECIFIED.,.F.,.F.)
B_SPLINE_CURVE_WITH_KNOTS((3,2,2,2,2,2,2,2,3),(0.795,0.7975,0.8,0.8025,
0.805,0.8075,0.81,0.8125,0.815),.UNSPECIFIED.)
CURVE()
GEOMETRIC_REPRESENTATION_ITEM()
RATIONAL_B_SPLINE_CURVE((1.,0.923879532511287,1.,0.923879532511287,1.,0.923879532511287,
1.,0.923879532511287,1.,0.923879532511287,1.,0.923879532511287,1.,0.923879532511287,
1.,0.923879532511287,1.))
REPRESENTATION_ITEM('')
);
#691=(
BOUNDED_CURVE()
B_SPLINE_CURVE(2,(#6164,#6165,#6166,#6167,#6168,#6169,#6170,#6171,#6172,
#6173,#6174,#6175,#6176,#6177,#6178,#6179,#6180),.UNSPECIFIED.,.F.,.F.)
B_SPLINE_CURVE_WITH_KNOTS((3,2,2,2,2,2,2,2,3),(0.775,0.7775,0.78,0.7825,
0.785,0.7875,0.79,0.7925,0.795),.UNSPECIFIED.)
CURVE()
GEOMETRIC_REPRESENTATION_ITEM()
RATIONAL_B_SPLINE_CURVE((1.,0.923879532511287,1.,0.923879532511287,1.,0.923879532511287,
1.,0.923879532511287,1.,0.923879532511287,1.,0.923879532511287,1.,0.923879532511287,
1.,0.923879532511287,1.))
REPRESENTATION_ITEM('')
);
#692=(
BOUNDED_CURVE()
B_SPLINE_CURVE(2,(#6185,#6186,#6187,#6188,#6189,#6190,#6191,#6192,#6193,
#6194,#6195,#6196,#6197,#6198,#6199,#6200,#6201),.UNSPECIFIED.,.F.,.F.)
B_SPLINE_CURVE_WITH_KNOTS((3,2,2,2,2,2,2,2,3),(0.775,0.7775,0.78,0.7825,
0.785,0.7875,0.79,0.7925,0.795),.UNSPECIFIED.)
CURVE()
GEOMETRIC_REPRESENTATION_ITEM()
RATIONAL_B_SPLINE_CURVE((1.,0.923879532511287,1.,0.923879532511287,1.,0.923879532511287,
1.,0.923879532511287,1.,0.923879532511287,1.,0.923879532511287,1.,0.923879532511287,
1.,0.923879532511287,1.))
REPRESENTATION_ITEM('')
);
#693=(
BOUNDED_CURVE()
B_SPLINE_CURVE(2,(#6202,#6203,#6204,#6205,#6206,#6207,#6208,#6209,#6210,
#6211,#6212,#6213,#6214,#6215,#6216,#6217,#6218),.UNSPECIFIED.,.F.,.F.)
B_SPLINE_CURVE_WITH_KNOTS((3,2,2,2,2,2,2,2,3),(0.755,0.7575,0.76,0.7625,
0.765,0.7675,0.77,0.7725,0.775),.UNSPECIFIED.)
CURVE()
GEOMETRIC_REPRESENTATION_ITEM()
RATIONAL_B_SPLINE_CURVE((1.,0.923879532511287,1.,0.923879532511287,1.,0.923879532511287,
1.,0.923879532511287,1.,0.923879532511287,1.,0.923879532511287,1.,0.923879532511287,
1.,0.923879532511287,1.))
REPRESENTATION_ITEM('')
);
#694=(
BOUNDED_CURVE()
B_SPLINE_CURVE(2,(#6223,#6224,#6225,#6226,#6227,#6228,#6229,#6230,#6231,
#6232,#6233,#6234,#6235,#6236,#6237,#6238,#6239),.UNSPECIFIED.,.F.,.F.)
B_SPLINE_CURVE_WITH_KNOTS((3,2,2,2,2,2,2,2,3),(0.755,0.7575,0.76,0.7625,
0.765,0.7675,0.77,0.7725,0.775),.UNSPECIFIED.)
CURVE()
GEOMETRIC_REPRESENTATION_ITEM()
RATIONAL_B_SPLINE_CURVE((1.,0.923879532511287,1.,0.923879532511287,1.,0.923879532511287,
1.,0.923879532511287,1.,0.923879532511287,1.,0.923879532511287,1.,0.923879532511287,
1.,0.923879532511287,1.))
REPRESENTATION_ITEM('')
);
#695=(
BOUNDED_CURVE()
B_SPLINE_CURVE(2,(#6240,#6241,#6242,#6243,#6244,#6245,#6246,#6247,#6248,
#6249,#6250,#6251,#6252,#6253,#6254,#6255,#6256),.UNSPECIFIED.,.F.,.F.)
B_SPLINE_CURVE_WITH_KNOTS((3,2,2,2,2,2,2,2,3),(0.735,0.7375,0.74,0.7425,
0.745,0.7475,0.75,0.7525,0.755),.UNSPECIFIED.)
CURVE()
GEOMETRIC_REPRESENTATION_ITEM()
RATIONAL_B_SPLINE_CURVE((1.,0.923879532511287,1.,0.923879532511287,1.,0.923879532511287,
1.,0.923879532511287,1.,0.923879532511287,1.,0.923879532511287,1.,0.923879532511287,
1.,0.923879532511287,1.))
REPRESENTATION_ITEM('')
);
#696=(
BOUNDED_CURVE()
B_SPLINE_CURVE(2,(#6261,#6262,#6263,#6264,#6265,#6266,#6267,#6268,#6269,
#6270,#6271,#6272,#6273,#6274,#6275,#6276,#6277),.UNSPECIFIED.,.F.,.F.)
B_SPLINE_CURVE_WITH_KNOTS((3,2,2,2,2,2,2,2,3),(0.735,0.7375,0.74,0.7425,
0.745,0.7475,0.75,0.7525,0.755),.UNSPECIFIED.)
CURVE()
GEOMETRIC_REPRESENTATION_ITEM()
RATIONAL_B_SPLINE_CURVE((1.,0.923879532511287,1.,0.923879532511287,1.,0.923879532511287,
1.,0.923879532511287,1.,0.923879532511287,1.,0.923879532511287,1.,0.923879532511287,
1.,0.923879532511287,1.))
REPRESENTATION_ITEM('')
);
#697=(
BOUNDED_CURVE()
B_SPLINE_CURVE(2,(#6278,#6279,#6280,#6281,#6282,#6283,#6284,#6285,#6286,
#6287,#6288,#6289,#6290,#6291,#6292,#6293,#6294),.UNSPECIFIED.,.F.,.F.)
B_SPLINE_CURVE_WITH_KNOTS((3,2,2,2,2,2,2,2,3),(0.715,0.7175,0.72,0.7225,
0.725,0.7275,0.73,0.7325,0.735),.UNSPECIFIED.)
CURVE()
GEOMETRIC_REPRESENTATION_ITEM()
RATIONAL_B_SPLINE_CURVE((1.,0.923879532511287,1.,0.923879532511287,1.,0.923879532511287,
1.,0.923879532511287,1.,0.923879532511287,1.,0.923879532511287,1.,0.923879532511287,
1.,0.923879532511287,1.))
REPRESENTATION_ITEM('')
);
#698=(
BOUNDED_CURVE()
B_SPLINE_CURVE(2,(#6299,#6300,#6301,#6302,#6303,#6304,#6305,#6306,#6307,
#6308,#6309,#6310,#6311,#6312,#6313,#6314,#6315),.UNSPECIFIED.,.F.,.F.)
B_SPLINE_CURVE_WITH_KNOTS((3,2,2,2,2,2,2,2,3),(0.715,0.7175,0.72,0.7225,
0.725,0.7275,0.73,0.7325,0.735),.UNSPECIFIED.)
CURVE()
GEOMETRIC_REPRESENTATION_ITEM()
RATIONAL_B_SPLINE_CURVE((1.,0.923879532511287,1.,0.923879532511287,1.,0.923879532511287,
1.,0.923879532511287,1.,0.923879532511287,1.,0.923879532511287,1.,0.923879532511287,
1.,0.923879532511287,1.))
REPRESENTATION_ITEM('')
);
#699=(
BOUNDED_CURVE()
B_SPLINE_CURVE(2,(#6316,#6317,#6318,#6319,#6320,#6321,#6322,#6323,#6324,
#6325,#6326,#6327,#6328,#6329,#6330,#6331,#6332),.UNSPECIFIED.,.F.,.F.)
B_SPLINE_CURVE_WITH_KNOTS((3,2,2,2,2,2,2,2,3),(0.695,0.6975,0.7,0.7025,
0.705,0.7075,0.71,0.7125,0.715),.UNSPECIFIED.)
CURVE()
GEOMETRIC_REPRESENTATION_ITEM()
RATIONAL_B_SPLINE_CURVE((1.,0.923879532511287,1.,0.923879532511287,1.,0.923879532511287,
1.,0.923879532511287,1.,0.923879532511287,1.,0.923879532511287,1.,0.923879532511287,
1.,0.923879532511287,1.))
REPRESENTATION_ITEM('')
);
#700=(
BOUNDED_CURVE()
B_SPLINE_CURVE(2,(#6337,#6338,#6339,#6340,#6341,#6342,#6343,#6344,#6345,
#6346,#6347,#6348,#6349,#6350,#6351,#6352,#6353),.UNSPECIFIED.,.F.,.F.)
B_SPLINE_CURVE_WITH_KNOTS((3,2,2,2,2,2,2,2,3),(0.695,0.6975,0.7,0.7025,
0.705,0.7075,0.71,0.7125,0.715),.UNSPECIFIED.)
CURVE()
GEOMETRIC_REPRESENTATION_ITEM()
RATIONAL_B_SPLINE_CURVE((1.,0.923879532511287,1.,0.923879532511287,1.,0.923879532511287,
1.,0.923879532511287,1.,0.923879532511287,1.,0.923879532511287,1.,0.923879532511287,
1.,0.923879532511287,1.))
REPRESENTATION_ITEM('')
);
#701=(
BOUNDED_CURVE()
B_SPLINE_CURVE(2,(#6354,#6355,#6356,#6357,#6358,#6359,#6360,#6361,#6362,
#6363,#6364,#6365,#6366,#6367,#6368,#6369,#6370),.UNSPECIFIED.,.F.,.F.)
B_SPLINE_CURVE_WITH_KNOTS((3,2,2,2,2,2,2,2,3),(0.675,0.6775,0.68,0.6825,
0.685,0.6875,0.69,0.6925,0.695),.UNSPECIFIED.)
CURVE()
GEOMETRIC_REPRESENTATION_ITEM()
RATIONAL_B_SPLINE_CURVE((1.,0.923879532511287,1.,0.923879532511287,1.,0.923879532511287,
1.,0.923879532511287,1.,0.923879532511287,1.,0.923879532511287,1.,0.923879532511287,
1.,0.923879532511287,1.))
REPRESENTATION_ITEM('')
);
#702=(
BOUNDED_CURVE()
B_SPLINE_CURVE(2,(#6375,#6376,#6377,#6378,#6379,#6380,#6381,#6382,#6383,
#6384,#6385,#6386,#6387,#6388,#6389,#6390,#6391),.UNSPECIFIED.,.F.,.F.)
B_SPLINE_CURVE_WITH_KNOTS((3,2,2,2,2,2,2,2,3),(0.675,0.6775,0.68,0.6825,
0.685,0.6875,0.69,0.6925,0.695),.UNSPECIFIED.)
CURVE()
GEOMETRIC_REPRESENTATION_ITEM()
RATIONAL_B_SPLINE_CURVE((1.,0.923879532511287,1.,0.923879532511287,1.,0.923879532511287,
1.,0.923879532511287,1.,0.923879532511287,1.,0.923879532511287,1.,0.923879532511287,
1.,0.923879532511287,1.))
REPRESENTATION_ITEM('')
);
#703=(
BOUNDED_CURVE()
B_SPLINE_CURVE(2,(#6392,#6393,#6394,#6395,#6396,#6397,#6398,#6399,#6400,
#6401,#6402,#6403,#6404,#6405,#6406,#6407,#6408),.UNSPECIFIED.,.F.,.F.)
B_SPLINE_CURVE_WITH_KNOTS((3,2,2,2,2,2,2,2,3),(0.655,0.6575,0.66,0.6625,
0.665,0.6675,0.67,0.6725,0.675),.UNSPECIFIED.)
CURVE()
GEOMETRIC_REPRESENTATION_ITEM()
RATIONAL_B_SPLINE_CURVE((1.,0.923879532511287,1.,0.923879532511287,1.,0.923879532511287,
1.,0.923879532511287,1.,0.923879532511287,1.,0.923879532511287,1.,0.923879532511287,
1.,0.923879532511287,1.))
REPRESENTATION_ITEM('')
);
#704=(
BOUNDED_CURVE()
B_SPLINE_CURVE(2,(#6413,#6414,#6415,#6416,#6417,#6418,#6419,#6420,#6421,
#6422,#6423,#6424,#6425,#6426,#6427,#6428,#6429),.UNSPECIFIED.,.F.,.F.)
B_SPLINE_CURVE_WITH_KNOTS((3,2,2,2,2,2,2,2,3),(0.655,0.6575,0.66,0.6625,
0.665,0.6675,0.67,0.6725,0.675),.UNSPECIFIED.)
CURVE()
GEOMETRIC_REPRESENTATION_ITEM()
RATIONAL_B_SPLINE_CURVE((1.,0.923879532511287,1.,0.923879532511287,1.,0.923879532511287,
1.,0.923879532511287,1.,0.923879532511287,1.,0.923879532511287,1.,0.923879532511287,
1.,0.923879532511287,1.))
REPRESENTATION_ITEM('')
);
#705=(
BOUNDED_CURVE()
B_SPLINE_CURVE(2,(#6430,#6431,#6432,#6433,#6434,#6435,#6436,#6437,#6438,
#6439,#6440,#6441,#6442,#6443,#6444,#6445,#6446),.UNSPECIFIED.,.F.,.F.)
B_SPLINE_CURVE_WITH_KNOTS((3,2,2,2,2,2,2,2,3),(0.635,0.6375,0.64,0.6425,
0.645,0.6475,0.65,0.6525,0.655),.UNSPECIFIED.)
CURVE()
GEOMETRIC_REPRESENTATION_ITEM()
RATIONAL_B_SPLINE_CURVE((1.,0.923879532511287,1.,0.923879532511287,1.,0.923879532511287,
1.,0.923879532511287,1.,0.923879532511287,1.,0.923879532511287,1.,0.923879532511287,
1.,0.923879532511287,1.))
REPRESENTATION_ITEM('')
);
#706=(
BOUNDED_CURVE()
B_SPLINE_CURVE(2,(#6451,#6452,#6453,#6454,#6455,#6456,#6457,#6458,#6459,
#6460,#6461,#6462,#6463,#6464,#6465,#6466,#6467),.UNSPECIFIED.,.F.,.F.)
B_SPLINE_CURVE_WITH_KNOTS((3,2,2,2,2,2,2,2,3),(0.635,0.6375,0.64,0.6425,
0.645,0.6475,0.65,0.6525,0.655),.UNSPECIFIED.)
CURVE()
GEOMETRIC_REPRESENTATION_ITEM()
RATIONAL_B_SPLINE_CURVE((1.,0.923879532511287,1.,0.923879532511287,1.,0.923879532511287,
1.,0.923879532511287,1.,0.923879532511287,1.,0.923879532511287,1.,0.923879532511287,
1.,0.923879532511287,1.))
REPRESENTATION_ITEM('')
);
#707=(
BOUNDED_CURVE()
B_SPLINE_CURVE(2,(#6468,#6469,#6470,#6471,#6472,#6473,#6474,#6475,#6476,
#6477,#6478,#6479,#6480,#6481,#6482,#6483,#6484),.UNSPECIFIED.,.F.,.F.)
B_SPLINE_CURVE_WITH_KNOTS((3,2,2,2,2,2,2,2,3),(0.615,0.6175,0.62,0.6225,
0.625,0.6275,0.63,0.6325,0.635),.UNSPECIFIED.)
CURVE()
GEOMETRIC_REPRESENTATION_ITEM()
RATIONAL_B_SPLINE_CURVE((1.,0.923879532511287,1.,0.923879532511287,1.,0.923879532511287,
1.,0.923879532511287,1.,0.923879532511287,1.,0.923879532511287,1.,0.923879532511287,
1.,0.923879532511287,1.))
REPRESENTATION_ITEM('')
);
#708=(
BOUNDED_CURVE()
B_SPLINE_CURVE(2,(#6489,#6490,#6491,#6492,#6493,#6494,#6495,#6496,#6497,
#6498,#6499,#6500,#6501,#6502,#6503,#6504,#6505),.UNSPECIFIED.,.F.,.F.)
B_SPLINE_CURVE_WITH_KNOTS((3,2,2,2,2,2,2,2,3),(0.615,0.6175,0.62,0.6225,
0.625,0.6275,0.63,0.6325,0.635),.UNSPECIFIED.)
CURVE()
GEOMETRIC_REPRESENTATION_ITEM()
RATIONAL_B_SPLINE_CURVE((1.,0.923879532511287,1.,0.923879532511287,1.,0.923879532511287,
1.,0.923879532511287,1.,0.923879532511287,1.,0.923879532511287,1.,0.923879532511287,
1.,0.923879532511287,1.))
REPRESENTATION_ITEM('')
);
#709=(
BOUNDED_CURVE()
B_SPLINE_CURVE(2,(#6506,#6507,#6508,#6509,#6510,#6511,#6512,#6513,#6514,
#6515,#6516,#6517,#6518,#6519,#6520,#6521,#6522),.UNSPECIFIED.,.F.,.F.)
B_SPLINE_CURVE_WITH_KNOTS((3,2,2,2,2,2,2,2,3),(0.595,0.5975,0.6,0.6025,
0.605,0.6075,0.61,0.6125,0.615),.UNSPECIFIED.)
CURVE()
GEOMETRIC_REPRESENTATION_ITEM()
RATIONAL_B_SPLINE_CURVE((1.,0.923879532511287,1.,0.923879532511287,1.,0.923879532511287,
1.,0.923879532511287,1.,0.923879532511287,1.,0.923879532511287,1.,0.923879532511287,
1.,0.923879532511287,1.))
REPRESENTATION_ITEM('')
);
#710=(
BOUNDED_CURVE()
B_SPLINE_CURVE(2,(#6527,#6528,#6529,#6530,#6531,#6532,#6533,#6534,#6535,
#6536,#6537,#6538,#6539,#6540,#6541,#6542,#6543),.UNSPECIFIED.,.F.,.F.)
B_SPLINE_CURVE_WITH_KNOTS((3,2,2,2,2,2,2,2,3),(0.595,0.5975,0.6,0.6025,
0.605,0.6075,0.61,0.6125,0.615),.UNSPECIFIED.)
CURVE()
GEOMETRIC_REPRESENTATION_ITEM()
RATIONAL_B_SPLINE_CURVE((1.,0.923879532511287,1.,0.923879532511287,1.,0.923879532511287,
1.,0.923879532511287,1.,0.923879532511287,1.,0.923879532511287,1.,0.923879532511287,
1.,0.923879532511287,1.))
REPRESENTATION_ITEM('')
);
#711=(
BOUNDED_CURVE()
B_SPLINE_CURVE(2,(#6544,#6545,#6546,#6547,#6548,#6549,#6550,#6551,#6552,
#6553,#6554,#6555,#6556,#6557,#6558,#6559,#6560),.UNSPECIFIED.,.F.,.F.)
B_SPLINE_CURVE_WITH_KNOTS((3,2,2,2,2,2,2,2,3),(0.575,0.5775,0.58,0.5825,
0.585,0.5875,0.59,0.5925,0.595),.UNSPECIFIED.)
CURVE()
GEOMETRIC_REPRESENTATION_ITEM()
RATIONAL_B_SPLINE_CURVE((1.,0.923879532511287,1.,0.923879532511287,1.,0.923879532511287,
1.,0.923879532511287,1.,0.923879532511287,1.,0.923879532511287,1.,0.923879532511287,
1.,0.923879532511287,1.))
REPRESENTATION_ITEM('')
);
#712=(
BOUNDED_CURVE()
B_SPLINE_CURVE(2,(#6565,#6566,#6567,#6568,#6569,#6570,#6571,#6572,#6573,
#6574,#6575,#6576,#6577,#6578,#6579,#6580,#6581),.UNSPECIFIED.,.F.,.F.)
B_SPLINE_CURVE_WITH_KNOTS((3,2,2,2,2,2,2,2,3),(0.575,0.5775,0.58,0.5825,
0.585,0.5875,0.59,0.5925,0.595),.UNSPECIFIED.)
CURVE()
GEOMETRIC_REPRESENTATION_ITEM()
RATIONAL_B_SPLINE_CURVE((1.,0.923879532511287,1.,0.923879532511287,1.,0.923879532511287,
1.,0.923879532511287,1.,0.923879532511287,1.,0.923879532511287,1.,0.923879532511287,
1.,0.923879532511287,1.))
REPRESENTATION_ITEM('')
);
#713=(
BOUNDED_CURVE()
B_SPLINE_CURVE(2,(#6582,#6583,#6584,#6585,#6586,#6587,#6588,#6589,#6590,
#6591,#6592,#6593,#6594,#6595,#6596,#6597,#6598),.UNSPECIFIED.,.F.,.F.)
B_SPLINE_CURVE_WITH_KNOTS((3,2,2,2,2,2,2,2,3),(0.555,0.5575,0.56,0.5625,
0.565,0.5675,0.57,0.5725,0.575),.UNSPECIFIED.)
CURVE()
GEOMETRIC_REPRESENTATION_ITEM()
RATIONAL_B_SPLINE_CURVE((1.,0.923879532511287,1.,0.923879532511287,1.,0.923879532511287,
1.,0.923879532511287,1.,0.923879532511287,1.,0.923879532511287,1.,0.923879532511287,
1.,0.923879532511287,1.))
REPRESENTATION_ITEM('')
);
#714=(
BOUNDED_CURVE()
B_SPLINE_CURVE(2,(#6603,#6604,#6605,#6606,#6607,#6608,#6609,#6610,#6611,
#6612,#6613,#6614,#6615,#6616,#6617,#6618,#6619),.UNSPECIFIED.,.F.,.F.)
B_SPLINE_CURVE_WITH_KNOTS((3,2,2,2,2,2,2,2,3),(0.555,0.5575,0.56,0.5625,
0.565,0.5675,0.57,0.5725,0.575),.UNSPECIFIED.)
CURVE()
GEOMETRIC_REPRESENTATION_ITEM()
RATIONAL_B_SPLINE_CURVE((1.,0.923879532511287,1.,0.923879532511287,1.,0.923879532511287,
1.,0.923879532511287,1.,0.923879532511287,1.,0.923879532511287,1.,0.923879532511287,
1.,0.923879532511287,1.))
REPRESENTATION_ITEM('')
);
#715=(
BOUNDED_CURVE()
B_SPLINE_CURVE(2,(#6620,#6621,#6622,#6623,#6624,#6625,#6626,#6627,#6628,
#6629,#6630,#6631,#6632,#6633,#6634,#6635,#6636),.UNSPECIFIED.,.F.,.F.)
B_SPLINE_CURVE_WITH_KNOTS((3,2,2,2,2,2,2,2,3),(0.535,0.5375,0.54,0.5425,
0.545,0.5475,0.55,0.5525,0.555),.UNSPECIFIED.)
CURVE()
GEOMETRIC_REPRESENTATION_ITEM()
RATIONAL_B_SPLINE_CURVE((1.,0.923879532511287,1.,0.923879532511287,1.,0.923879532511287,
1.,0.923879532511287,1.,0.923879532511287,1.,0.923879532511287,1.,0.923879532511287,
1.,0.923879532511287,1.))
REPRESENTATION_ITEM('')
);
#716=(
BOUNDED_CURVE()
B_SPLINE_CURVE(2,(#6641,#6642,#6643,#6644,#6645,#6646,#6647,#6648,#6649,
#6650,#6651,#6652,#6653,#6654,#6655,#6656,#6657),.UNSPECIFIED.,.F.,.F.)
B_SPLINE_CURVE_WITH_KNOTS((3,2,2,2,2,2,2,2,3),(0.535,0.5375,0.54,0.5425,
0.545,0.5475,0.55,0.5525,0.555),.UNSPECIFIED.)
CURVE()
GEOMETRIC_REPRESENTATION_ITEM()
RATIONAL_B_SPLINE_CURVE((1.,0.923879532511287,1.,0.923879532511287,1.,0.923879532511287,
1.,0.923879532511287,1.,0.923879532511287,1.,0.923879532511287,1.,0.923879532511287,
1.,0.923879532511287,1.))
REPRESENTATION_ITEM('')
);
#717=(
BOUNDED_CURVE()
B_SPLINE_CURVE(2,(#6658,#6659,#6660,#6661,#6662,#6663,#6664,#6665,#6666,
#6667,#6668,#6669,#6670,#6671,#6672,#6673,#6674),.UNSPECIFIED.,.F.,.F.)
B_SPLINE_CURVE_WITH_KNOTS((3,2,2,2,2,2,2,2,3),(0.515,0.5175,0.52,0.5225,
0.525,0.5275,0.53,0.5325,0.535),.UNSPECIFIED.)
CURVE()
GEOMETRIC_REPRESENTATION_ITEM()
RATIONAL_B_SPLINE_CURVE((1.,0.923879532511287,1.,0.923879532511287,1.,0.923879532511287,
1.,0.923879532511287,1.,0.923879532511287,1.,0.923879532511287,1.,0.923879532511287,
1.,0.923879532511287,1.))
REPRESENTATION_ITEM('')
);
#718=(
BOUNDED_CURVE()
B_SPLINE_CURVE(2,(#6679,#6680,#6681,#6682,#6683,#6684,#6685,#6686,#6687,
#6688,#6689,#6690,#6691,#6692,#6693,#6694,#6695),.UNSPECIFIED.,.F.,.F.)
B_SPLINE_CURVE_WITH_KNOTS((3,2,2,2,2,2,2,2,3),(0.515,0.5175,0.52,0.5225,
0.525,0.5275,0.53,0.5325,0.535),.UNSPECIFIED.)
CURVE()
GEOMETRIC_REPRESENTATION_ITEM()
RATIONAL_B_SPLINE_CURVE((1.,0.923879532511287,1.,0.923879532511287,1.,0.923879532511287,
1.,0.923879532511287,1.,0.923879532511287,1.,0.923879532511287,1.,0.923879532511287,
1.,0.923879532511287,1.))
REPRESENTATION_ITEM('')
);
#719=(
BOUNDED_CURVE()
B_SPLINE_CURVE(2,(#6696,#6697,#6698,#6699,#6700,#6701,#6702,#6703,#6704,
#6705,#6706,#6707,#6708,#6709,#6710,#6711,#6712),.UNSPECIFIED.,.F.,.F.)
B_SPLINE_CURVE_WITH_KNOTS((3,2,2,2,2,2,2,2,3),(0.495,0.4975,0.5,0.5025,
0.505,0.5075,0.51,0.5125,0.515),.UNSPECIFIED.)
CURVE()
GEOMETRIC_REPRESENTATION_ITEM()
RATIONAL_B_SPLINE_CURVE((1.,0.923879532511287,1.,0.923879532511287,1.,0.923879532511287,
1.,0.923879532511287,1.,0.923879532511287,1.,0.923879532511287,1.,0.923879532511287,
1.,0.923879532511287,1.))
REPRESENTATION_ITEM('')
);
#720=(
BOUNDED_CURVE()
B_SPLINE_CURVE(2,(#6717,#6718,#6719,#6720,#6721,#6722,#6723,#6724,#6725,
#6726,#6727,#6728,#6729,#6730,#6731,#6732,#6733),.UNSPECIFIED.,.F.,.F.)
B_SPLINE_CURVE_WITH_KNOTS((3,2,2,2,2,2,2,2,3),(0.495,0.4975,0.5,0.5025,
0.505,0.5075,0.51,0.5125,0.515),.UNSPECIFIED.)
CURVE()
GEOMETRIC_REPRESENTATION_ITEM()
RATIONAL_B_SPLINE_CURVE((1.,0.923879532511287,1.,0.923879532511287,1.,0.923879532511287,
1.,0.923879532511287,1.,0.923879532511287,1.,0.923879532511287,1.,0.923879532511287,
1.,0.923879532511287,1.))
REPRESENTATION_ITEM('')
);
#721=(
BOUNDED_CURVE()
B_SPLINE_CURVE(2,(#6734,#6735,#6736,#6737,#6738,#6739,#6740,#6741,#6742,
#6743,#6744,#6745,#6746,#6747,#6748,#6749,#6750),.UNSPECIFIED.,.F.,.F.)
B_SPLINE_CURVE_WITH_KNOTS((3,2,2,2,2,2,2,2,3),(0.475,0.4775,0.48,0.4825,
0.485,0.4875,0.49,0.4925,0.495),.UNSPECIFIED.)
CURVE()
GEOMETRIC_REPRESENTATION_ITEM()
RATIONAL_B_SPLINE_CURVE((1.,0.923879532511287,1.,0.923879532511287,1.,0.923879532511287,
1.,0.923879532511287,1.,0.923879532511287,1.,0.923879532511287,1.,0.923879532511287,
1.,0.923879532511287,1.))
REPRESENTATION_ITEM('')
);
#722=(
BOUNDED_CURVE()
B_SPLINE_CURVE(2,(#6755,#6756,#6757,#6758,#6759,#6760,#6761,#6762,#6763,
#6764,#6765,#6766,#6767,#6768,#6769,#6770,#6771),.UNSPECIFIED.,.F.,.F.)
B_SPLINE_CURVE_WITH_KNOTS((3,2,2,2,2,2,2,2,3),(0.475,0.4775,0.48,0.4825,
0.485,0.4875,0.49,0.4925,0.495),.UNSPECIFIED.)
CURVE()
GEOMETRIC_REPRESENTATION_ITEM()
RATIONAL_B_SPLINE_CURVE((1.,0.923879532511287,1.,0.923879532511287,1.,0.923879532511287,
1.,0.923879532511287,1.,0.923879532511287,1.,0.923879532511287,1.,0.923879532511287,
1.,0.923879532511287,1.))
REPRESENTATION_ITEM('')
);
#723=(
BOUNDED_CURVE()
B_SPLINE_CURVE(2,(#6772,#6773,#6774,#6775,#6776,#6777,#6778,#6779,#6780,
#6781,#6782,#6783,#6784,#6785,#6786,#6787,#6788),.UNSPECIFIED.,.F.,.F.)
B_SPLINE_CURVE_WITH_KNOTS((3,2,2,2,2,2,2,2,3),(0.455,0.4575,0.46,0.4625,
0.465,0.4675,0.47,0.4725,0.475),.UNSPECIFIED.)
CURVE()
GEOMETRIC_REPRESENTATION_ITEM()
RATIONAL_B_SPLINE_CURVE((1.,0.923879532511287,1.,0.923879532511287,1.,0.923879532511287,
1.,0.923879532511287,1.,0.923879532511287,1.,0.923879532511287,1.,0.923879532511287,
1.,0.923879532511287,1.))
REPRESENTATION_ITEM('')
);
#724=(
BOUNDED_CURVE()
B_SPLINE_CURVE(2,(#6793,#6794,#6795,#6796,#6797,#6798,#6799,#6800,#6801,
#6802,#6803,#6804,#6805,#6806,#6807,#6808,#6809),.UNSPECIFIED.,.F.,.F.)
B_SPLINE_CURVE_WITH_KNOTS((3,2,2,2,2,2,2,2,3),(0.455,0.4575,0.46,0.4625,
0.465,0.4675,0.47,0.4725,0.475),.UNSPECIFIED.)
CURVE()
GEOMETRIC_REPRESENTATION_ITEM()
RATIONAL_B_SPLINE_CURVE((1.,0.923879532511287,1.,0.923879532511287,1.,0.923879532511287,
1.,0.923879532511287,1.,0.923879532511287,1.,0.923879532511287,1.,0.923879532511287,
1.,0.923879532511287,1.))
REPRESENTATION_ITEM('')
);
#725=(
BOUNDED_CURVE()
B_SPLINE_CURVE(2,(#6810,#6811,#6812,#6813,#6814,#6815,#6816,#6817,#6818,
#6819,#6820,#6821,#6822,#6823,#6824,#6825,#6826),.UNSPECIFIED.,.F.,.F.)
B_SPLINE_CURVE_WITH_KNOTS((3,2,2,2,2,2,2,2,3),(0.435,0.4375,0.44,0.4425,
0.445,0.4475,0.45,0.4525,0.455),.UNSPECIFIED.)
CURVE()
GEOMETRIC_REPRESENTATION_ITEM()
RATIONAL_B_SPLINE_CURVE((1.,0.923879532511287,1.,0.923879532511287,1.,0.923879532511287,
1.,0.923879532511287,1.,0.923879532511287,1.,0.923879532511287,1.,0.923879532511287,
1.,0.923879532511287,1.))
REPRESENTATION_ITEM('')
);
#726=(
BOUNDED_CURVE()
B_SPLINE_CURVE(2,(#6831,#6832,#6833,#6834,#6835,#6836,#6837,#6838,#6839,
#6840,#6841,#6842,#6843,#6844,#6845,#6846,#6847),.UNSPECIFIED.,.F.,.F.)
B_SPLINE_CURVE_WITH_KNOTS((3,2,2,2,2,2,2,2,3),(0.435,0.4375,0.44,0.4425,
0.445,0.4475,0.45,0.4525,0.455),.UNSPECIFIED.)
CURVE()
GEOMETRIC_REPRESENTATION_ITEM()
RATIONAL_B_SPLINE_CURVE((1.,0.923879532511287,1.,0.923879532511287,1.,0.923879532511287,
1.,0.923879532511287,1.,0.923879532511287,1.,0.923879532511287,1.,0.923879532511287,
1.,0.923879532511287,1.))
REPRESENTATION_ITEM('')
);
#727=(
BOUNDED_CURVE()
B_SPLINE_CURVE(2,(#6848,#6849,#6850,#6851,#6852,#6853,#6854,#6855,#6856,
#6857,#6858,#6859,#6860,#6861,#6862,#6863,#6864),.UNSPECIFIED.,.F.,.F.)
B_SPLINE_CURVE_WITH_KNOTS((3,2,2,2,2,2,2,2,3),(0.415,0.4175,0.42,0.4225,
0.425,0.4275,0.43,0.4325,0.435),.UNSPECIFIED.)
CURVE()
GEOMETRIC_REPRESENTATION_ITEM()
RATIONAL_B_SPLINE_CURVE((1.,0.923879532511287,1.,0.923879532511287,1.,0.923879532511287,
1.,0.923879532511287,1.,0.923879532511287,1.,0.923879532511287,1.,0.923879532511287,
1.,0.923879532511287,1.))
REPRESENTATION_ITEM('')
);
#728=(
BOUNDED_CURVE()
B_SPLINE_CURVE(2,(#6869,#6870,#6871,#6872,#6873,#6874,#6875,#6876,#6877,
#6878,#6879,#6880,#6881,#6882,#6883,#6884,#6885),.UNSPECIFIED.,.F.,.F.)
B_SPLINE_CURVE_WITH_KNOTS((3,2,2,2,2,2,2,2,3),(0.415,0.4175,0.42,0.4225,
0.425,0.4275,0.43,0.4325,0.435),.UNSPECIFIED.)
CURVE()
GEOMETRIC_REPRESENTATION_ITEM()
RATIONAL_B_SPLINE_CURVE((1.,0.923879532511287,1.,0.923879532511287,1.,0.923879532511287,
1.,0.923879532511287,1.,0.923879532511287,1.,0.923879532511287,1.,0.923879532511287,
1.,0.923879532511287,1.))
REPRESENTATION_ITEM('')
);
#729=(
BOUNDED_CURVE()
B_SPLINE_CURVE(2,(#6886,#6887,#6888,#6889,#6890,#6891,#6892,#6893,#6894,
#6895,#6896,#6897,#6898,#6899,#6900,#6901,#6902),.UNSPECIFIED.,.F.,.F.)
B_SPLINE_CURVE_WITH_KNOTS((3,2,2,2,2,2,2,2,3),(0.395,0.3975,0.4,0.4025,
0.405,0.4075,0.41,0.4125,0.415),.UNSPECIFIED.)
CURVE()
GEOMETRIC_REPRESENTATION_ITEM()
RATIONAL_B_SPLINE_CURVE((1.,0.923879532511287,1.,0.923879532511287,1.,0.923879532511287,
1.,0.923879532511287,1.,0.923879532511287,1.,0.923879532511287,1.,0.923879532511287,
1.,0.923879532511287,1.))
REPRESENTATION_ITEM('')
);
#730=(
BOUNDED_CURVE()
B_SPLINE_CURVE(2,(#6907,#6908,#6909,#6910,#6911,#6912,#6913,#6914,#6915,
#6916,#6917,#6918,#6919,#6920,#6921,#6922,#6923),.UNSPECIFIED.,.F.,.F.)
B_SPLINE_CURVE_WITH_KNOTS((3,2,2,2,2,2,2,2,3),(0.395,0.3975,0.4,0.4025,
0.405,0.4075,0.41,0.4125,0.415),.UNSPECIFIED.)
CURVE()
GEOMETRIC_REPRESENTATION_ITEM()
RATIONAL_B_SPLINE_CURVE((1.,0.923879532511287,1.,0.923879532511287,1.,0.923879532511287,
1.,0.923879532511287,1.,0.923879532511287,1.,0.923879532511287,1.,0.923879532511287,
1.,0.923879532511287,1.))
REPRESENTATION_ITEM('')
);
#731=(
BOUNDED_CURVE()
B_SPLINE_CURVE(2,(#6924,#6925,#6926,#6927,#6928,#6929,#6930,#6931,#6932,
#6933,#6934,#6935,#6936,#6937,#6938,#6939,#6940),.UNSPECIFIED.,.F.,.F.)
B_SPLINE_CURVE_WITH_KNOTS((3,2,2,2,2,2,2,2,3),(0.375,0.3775,0.38,0.3825,
0.385,0.3875,0.39,0.3925,0.395),.UNSPECIFIED.)
CURVE()
GEOMETRIC_REPRESENTATION_ITEM()
RATIONAL_B_SPLINE_CURVE((1.,0.923879532511287,1.,0.923879532511287,1.,0.923879532511287,
1.,0.923879532511287,1.,0.923879532511287,1.,0.923879532511287,1.,0.923879532511287,
1.,0.923879532511287,1.))
REPRESENTATION_ITEM('')
);
#732=(
BOUNDED_CURVE()
B_SPLINE_CURVE(2,(#6945,#6946,#6947,#6948,#6949,#6950,#6951,#6952,#6953,
#6954,#6955,#6956,#6957,#6958,#6959,#6960,#6961),.UNSPECIFIED.,.F.,.F.)
B_SPLINE_CURVE_WITH_KNOTS((3,2,2,2,2,2,2,2,3),(0.375,0.3775,0.38,0.3825,
0.385,0.3875,0.39,0.3925,0.395),.UNSPECIFIED.)
CURVE()
GEOMETRIC_REPRESENTATION_ITEM()
RATIONAL_B_SPLINE_CURVE((1.,0.923879532511287,1.,0.923879532511287,1.,0.923879532511287,
1.,0.923879532511287,1.,0.923879532511287,1.,0.923879532511287,1.,0.923879532511287,
1.,0.923879532511287,1.))
REPRESENTATION_ITEM('')
);
#733=(
BOUNDED_CURVE()
B_SPLINE_CURVE(2,(#6962,#6963,#6964,#6965,#6966,#6967,#6968,#6969,#6970,
#6971,#6972,#6973,#6974,#6975,#6976,#6977,#6978),.UNSPECIFIED.,.F.,.F.)
B_SPLINE_CURVE_WITH_KNOTS((3,2,2,2,2,2,2,2,3),(0.355,0.3575,0.36,0.3625,
0.365,0.3675,0.37,0.3725,0.375),.UNSPECIFIED.)
CURVE()
GEOMETRIC_REPRESENTATION_ITEM()
RATIONAL_B_SPLINE_CURVE((1.,0.923879532511287,1.,0.923879532511287,1.,0.923879532511287,
1.,0.923879532511287,1.,0.923879532511287,1.,0.923879532511287,1.,0.923879532511287,
1.,0.923879532511287,1.))
REPRESENTATION_ITEM('')
);
#734=(
BOUNDED_CURVE()
B_SPLINE_CURVE(2,(#6983,#6984,#6985,#6986,#6987,#6988,#6989,#6990,#6991,
#6992,#6993,#6994,#6995,#6996,#6997,#6998,#6999),.UNSPECIFIED.,.F.,.F.)
B_SPLINE_CURVE_WITH_KNOTS((3,2,2,2,2,2,2,2,3),(0.355,0.3575,0.36,0.3625,
0.365,0.3675,0.37,0.3725,0.375),.UNSPECIFIED.)
CURVE()
GEOMETRIC_REPRESENTATION_ITEM()
RATIONAL_B_SPLINE_CURVE((1.,0.923879532511287,1.,0.923879532511287,1.,0.923879532511287,
1.,0.923879532511287,1.,0.923879532511287,1.,0.923879532511287,1.,0.923879532511287,
1.,0.923879532511287,1.))
REPRESENTATION_ITEM('')
);
#735=(
BOUNDED_CURVE()
B_SPLINE_CURVE(2,(#7000,#7001,#7002,#7003,#7004,#7005,#7006,#7007,#7008,
#7009,#7010,#7011,#7012,#7013,#7014,#7015,#7016),.UNSPECIFIED.,.F.,.F.)
B_SPLINE_CURVE_WITH_KNOTS((3,2,2,2,2,2,2,2,3),(0.335,0.3375,0.34,0.3425,
0.345,0.3475,0.35,0.3525,0.355),.UNSPECIFIED.)
CURVE()
GEOMETRIC_REPRESENTATION_ITEM()
RATIONAL_B_SPLINE_CURVE((1.,0.923879532511287,1.,0.923879532511287,1.,0.923879532511287,
1.,0.923879532511287,1.,0.923879532511287,1.,0.923879532511287,1.,0.923879532511287,
1.,0.923879532511287,1.))
REPRESENTATION_ITEM('')
);
#736=(
BOUNDED_CURVE()
B_SPLINE_CURVE(2,(#7021,#7022,#7023,#7024,#7025,#7026,#7027,#7028,#7029,
#7030,#7031,#7032,#7033,#7034,#7035,#7036,#7037),.UNSPECIFIED.,.F.,.F.)
B_SPLINE_CURVE_WITH_KNOTS((3,2,2,2,2,2,2,2,3),(0.335,0.3375,0.34,0.3425,
0.345,0.3475,0.35,0.3525,0.355),.UNSPECIFIED.)
CURVE()
GEOMETRIC_REPRESENTATION_ITEM()
RATIONAL_B_SPLINE_CURVE((1.,0.923879532511287,1.,0.923879532511287,1.,0.923879532511287,
1.,0.923879532511287,1.,0.923879532511287,1.,0.923879532511287,1.,0.923879532511287,
1.,0.923879532511287,1.))
REPRESENTATION_ITEM('')
);
#737=(
BOUNDED_CURVE()
B_SPLINE_CURVE(2,(#7038,#7039,#7040,#7041,#7042,#7043,#7044,#7045,#7046,
#7047,#7048,#7049,#7050,#7051,#7052,#7053,#7054),.UNSPECIFIED.,.F.,.F.)
B_SPLINE_CURVE_WITH_KNOTS((3,2,2,2,2,2,2,2,3),(0.315,0.3175,0.32,0.3225,
0.325,0.3275,0.33,0.3325,0.335),.UNSPECIFIED.)
CURVE()
GEOMETRIC_REPRESENTATION_ITEM()
RATIONAL_B_SPLINE_CURVE((1.,0.923879532511287,1.,0.923879532511287,1.,0.923879532511287,
1.,0.923879532511287,1.,0.923879532511287,1.,0.923879532511287,1.,0.923879532511287,
1.,0.923879532511287,1.))
REPRESENTATION_ITEM('')
);
#738=(
BOUNDED_CURVE()
B_SPLINE_CURVE(2,(#7059,#7060,#7061,#7062,#7063,#7064,#7065,#7066,#7067,
#7068,#7069,#7070,#7071,#7072,#7073,#7074,#7075),.UNSPECIFIED.,.F.,.F.)
B_SPLINE_CURVE_WITH_KNOTS((3,2,2,2,2,2,2,2,3),(0.315,0.3175,0.32,0.3225,
0.325,0.3275,0.33,0.3325,0.335),.UNSPECIFIED.)
CURVE()
GEOMETRIC_REPRESENTATION_ITEM()
RATIONAL_B_SPLINE_CURVE((1.,0.923879532511287,1.,0.923879532511287,1.,0.923879532511287,
1.,0.923879532511287,1.,0.923879532511287,1.,0.923879532511287,1.,0.923879532511287,
1.,0.923879532511287,1.))
REPRESENTATION_ITEM('')
);
#739=(
BOUNDED_CURVE()
B_SPLINE_CURVE(2,(#7076,#7077,#7078,#7079,#7080,#7081,#7082,#7083,#7084,
#7085,#7086,#7087,#7088,#7089,#7090,#7091,#7092),.UNSPECIFIED.,.F.,.F.)
B_SPLINE_CURVE_WITH_KNOTS((3,2,2,2,2,2,2,2,3),(0.295,0.2975,0.3,0.3025,
0.305,0.3075,0.31,0.3125,0.315),.UNSPECIFIED.)
CURVE()
GEOMETRIC_REPRESENTATION_ITEM()
RATIONAL_B_SPLINE_CURVE((1.,0.923879532511287,1.,0.923879532511287,1.,0.923879532511287,
1.,0.923879532511287,1.,0.923879532511287,1.,0.923879532511287,1.,0.923879532511287,
1.,0.923879532511287,1.))
REPRESENTATION_ITEM('')
);
#740=(
BOUNDED_CURVE()
B_SPLINE_CURVE(2,(#7097,#7098,#7099,#7100,#7101,#7102,#7103,#7104,#7105,
#7106,#7107,#7108,#7109,#7110,#7111,#7112,#7113),.UNSPECIFIED.,.F.,.F.)
B_SPLINE_CURVE_WITH_KNOTS((3,2,2,2,2,2,2,2,3),(0.295,0.2975,0.3,0.3025,
0.305,0.3075,0.31,0.3125,0.315),.UNSPECIFIED.)
CURVE()
GEOMETRIC_REPRESENTATION_ITEM()
RATIONAL_B_SPLINE_CURVE((1.,0.923879532511287,1.,0.923879532511287,1.,0.923879532511287,
1.,0.923879532511287,1.,0.923879532511287,1.,0.923879532511287,1.,0.923879532511287,
1.,0.923879532511287,1.))
REPRESENTATION_ITEM('')
);
#741=(
BOUNDED_CURVE()
B_SPLINE_CURVE(2,(#7114,#7115,#7116,#7117,#7118,#7119,#7120,#7121,#7122,
#7123,#7124,#7125,#7126,#7127,#7128,#7129,#7130),.UNSPECIFIED.,.F.,.F.)
B_SPLINE_CURVE_WITH_KNOTS((3,2,2,2,2,2,2,2,3),(0.275,0.2775,0.28,0.2825,
0.285,0.2875,0.29,0.2925,0.295),.UNSPECIFIED.)
CURVE()
GEOMETRIC_REPRESENTATION_ITEM()
RATIONAL_B_SPLINE_CURVE((1.,0.923879532511287,1.,0.923879532511287,1.,0.923879532511287,
1.,0.923879532511287,1.,0.923879532511287,1.,0.923879532511287,1.,0.923879532511287,
1.,0.923879532511287,1.))
REPRESENTATION_ITEM('')
);
#742=(
BOUNDED_CURVE()
B_SPLINE_CURVE(2,(#7135,#7136,#7137,#7138,#7139,#7140,#7141,#7142,#7143,
#7144,#7145,#7146,#7147,#7148,#7149,#7150,#7151),.UNSPECIFIED.,.F.,.F.)
B_SPLINE_CURVE_WITH_KNOTS((3,2,2,2,2,2,2,2,3),(0.275,0.2775,0.28,0.2825,
0.285,0.2875,0.29,0.2925,0.295),.UNSPECIFIED.)
CURVE()
GEOMETRIC_REPRESENTATION_ITEM()
RATIONAL_B_SPLINE_CURVE((1.,0.923879532511287,1.,0.923879532511287,1.,0.923879532511287,
1.,0.923879532511287,1.,0.923879532511287,1.,0.923879532511287,1.,0.923879532511287,
1.,0.923879532511287,1.))
REPRESENTATION_ITEM('')
);
#743=(
BOUNDED_CURVE()
B_SPLINE_CURVE(2,(#7152,#7153,#7154,#7155,#7156,#7157,#7158,#7159,#7160,
#7161,#7162,#7163,#7164,#7165,#7166,#7167,#7168),.UNSPECIFIED.,.F.,.F.)
B_SPLINE_CURVE_WITH_KNOTS((3,2,2,2,2,2,2,2,3),(0.255,0.2575,0.26,0.2625,
0.265,0.2675,0.27,0.2725,0.275),.UNSPECIFIED.)
CURVE()
GEOMETRIC_REPRESENTATION_ITEM()
RATIONAL_B_SPLINE_CURVE((1.,0.923879532511287,1.,0.923879532511287,1.,0.923879532511287,
1.,0.923879532511287,1.,0.923879532511287,1.,0.923879532511287,1.,0.923879532511287,
1.,0.923879532511287,1.))
REPRESENTATION_ITEM('')
);
#744=(
BOUNDED_CURVE()
B_SPLINE_CURVE(2,(#7173,#7174,#7175,#7176,#7177,#7178,#7179,#7180,#7181,
#7182,#7183,#7184,#7185,#7186,#7187,#7188,#7189),.UNSPECIFIED.,.F.,.F.)
B_SPLINE_CURVE_WITH_KNOTS((3,2,2,2,2,2,2,2,3),(0.255,0.2575,0.26,0.2625,
0.265,0.2675,0.27,0.2725,0.275),.UNSPECIFIED.)
CURVE()
GEOMETRIC_REPRESENTATION_ITEM()
RATIONAL_B_SPLINE_CURVE((1.,0.923879532511287,1.,0.923879532511287,1.,0.923879532511287,
1.,0.923879532511287,1.,0.923879532511287,1.,0.923879532511287,1.,0.923879532511287,
1.,0.923879532511287,1.))
REPRESENTATION_ITEM('')
);
#745=(
BOUNDED_CURVE()
B_SPLINE_CURVE(2,(#7190,#7191,#7192,#7193,#7194,#7195,#7196,#7197,#7198,
#7199,#7200,#7201,#7202,#7203,#7204,#7205,#7206),.UNSPECIFIED.,.F.,.F.)
B_SPLINE_CURVE_WITH_KNOTS((3,2,2,2,2,2,2,2,3),(0.235,0.2375,0.24,0.2425,
0.245,0.2475,0.25,0.2525,0.255),.UNSPECIFIED.)
CURVE()
GEOMETRIC_REPRESENTATION_ITEM()
RATIONAL_B_SPLINE_CURVE((1.,0.923879532511287,1.,0.923879532511287,1.,0.923879532511287,
1.,0.923879532511287,1.,0.923879532511287,1.,0.923879532511287,1.,0.923879532511287,
1.,0.923879532511287,1.))
REPRESENTATION_ITEM('')
);
#746=(
BOUNDED_CURVE()
B_SPLINE_CURVE(2,(#7211,#7212,#7213,#7214,#7215,#7216,#7217,#7218,#7219,
#7220,#7221,#7222,#7223,#7224,#7225,#7226,#7227),.UNSPECIFIED.,.F.,.F.)
B_SPLINE_CURVE_WITH_KNOTS((3,2,2,2,2,2,2,2,3),(0.235,0.2375,0.24,0.2425,
0.245,0.2475,0.25,0.2525,0.255),.UNSPECIFIED.)
CURVE()
GEOMETRIC_REPRESENTATION_ITEM()
RATIONAL_B_SPLINE_CURVE((1.,0.923879532511287,1.,0.923879532511287,1.,0.923879532511287,
1.,0.923879532511287,1.,0.923879532511287,1.,0.923879532511287,1.,0.923879532511287,
1.,0.923879532511287,1.))
REPRESENTATION_ITEM('')
);
#747=(
BOUNDED_CURVE()
B_SPLINE_CURVE(2,(#7228,#7229,#7230,#7231,#7232,#7233,#7234,#7235,#7236,
#7237,#7238,#7239,#7240,#7241,#7242,#7243,#7244),.UNSPECIFIED.,.F.,.F.)
B_SPLINE_CURVE_WITH_KNOTS((3,2,2,2,2,2,2,2,3),(0.215,0.2175,0.22,0.2225,
0.225,0.2275,0.23,0.2325,0.235),.UNSPECIFIED.)
CURVE()
GEOMETRIC_REPRESENTATION_ITEM()
RATIONAL_B_SPLINE_CURVE((1.,0.923879532511287,1.,0.923879532511287,1.,0.923879532511287,
1.,0.923879532511287,1.,0.923879532511287,1.,0.923879532511287,1.,0.923879532511287,
1.,0.923879532511287,1.))
REPRESENTATION_ITEM('')
);
#748=(
BOUNDED_CURVE()
B_SPLINE_CURVE(2,(#7249,#7250,#7251,#7252,#7253,#7254,#7255,#7256,#7257,
#7258,#7259,#7260,#7261,#7262,#7263,#7264,#7265),.UNSPECIFIED.,.F.,.F.)
B_SPLINE_CURVE_WITH_KNOTS((3,2,2,2,2,2,2,2,3),(0.215,0.2175,0.22,0.2225,
0.225,0.2275,0.23,0.2325,0.235),.UNSPECIFIED.)
CURVE()
GEOMETRIC_REPRESENTATION_ITEM()
RATIONAL_B_SPLINE_CURVE((1.,0.923879532511287,1.,0.923879532511287,1.,0.923879532511287,
1.,0.923879532511287,1.,0.923879532511287,1.,0.923879532511287,1.,0.923879532511287,
1.,0.923879532511287,1.))
REPRESENTATION_ITEM('')
);
#749=(
BOUNDED_CURVE()
B_SPLINE_CURVE(2,(#7266,#7267,#7268,#7269,#7270,#7271,#7272,#7273,#7274,
#7275,#7276,#7277,#7278,#7279,#7280,#7281,#7282),.UNSPECIFIED.,.F.,.F.)
B_SPLINE_CURVE_WITH_KNOTS((3,2,2,2,2,2,2,2,3),(0.195,0.1975,0.2,0.2025,
0.205,0.2075,0.21,0.2125,0.215),.UNSPECIFIED.)
CURVE()
GEOMETRIC_REPRESENTATION_ITEM()
RATIONAL_B_SPLINE_CURVE((1.,0.923879532511287,1.,0.923879532511287,1.,0.923879532511287,
1.,0.923879532511287,1.,0.923879532511287,1.,0.923879532511287,1.,0.923879532511287,
1.,0.923879532511287,1.))
REPRESENTATION_ITEM('')
);
#750=(
BOUNDED_CURVE()
B_SPLINE_CURVE(2,(#7287,#7288,#7289,#7290,#7291,#7292,#7293,#7294,#7295,
#7296,#7297,#7298,#7299,#7300,#7301,#7302,#7303),.UNSPECIFIED.,.F.,.F.)
B_SPLINE_CURVE_WITH_KNOTS((3,2,2,2,2,2,2,2,3),(0.195,0.1975,0.2,0.2025,
0.205,0.2075,0.21,0.2125,0.215),.UNSPECIFIED.)
CURVE()
GEOMETRIC_REPRESENTATION_ITEM()
RATIONAL_B_SPLINE_CURVE((1.,0.923879532511287,1.,0.923879532511287,1.,0.923879532511287,
1.,0.923879532511287,1.,0.923879532511287,1.,0.923879532511287,1.,0.923879532511287,
1.,0.923879532511287,1.))
REPRESENTATION_ITEM('')
);
#751=(
BOUNDED_CURVE()
B_SPLINE_CURVE(2,(#7304,#7305,#7306,#7307,#7308,#7309,#7310,#7311,#7312,
#7313,#7314,#7315,#7316,#7317,#7318,#7319,#7320),.UNSPECIFIED.,.F.,.F.)
B_SPLINE_CURVE_WITH_KNOTS((3,2,2,2,2,2,2,2,3),(0.175,0.1775,0.18,0.1825,
0.185,0.1875,0.19,0.1925,0.195),.UNSPECIFIED.)
CURVE()
GEOMETRIC_REPRESENTATION_ITEM()
RATIONAL_B_SPLINE_CURVE((1.,0.923879532511287,1.,0.923879532511287,1.,0.923879532511287,
1.,0.923879532511287,1.,0.923879532511287,1.,0.923879532511287,1.,0.923879532511287,
1.,0.923879532511287,1.))
REPRESENTATION_ITEM('')
);
#752=(
BOUNDED_CURVE()
B_SPLINE_CURVE(2,(#7325,#7326,#7327,#7328,#7329,#7330,#7331,#7332,#7333,
#7334,#7335,#7336,#7337,#7338,#7339,#7340,#7341),.UNSPECIFIED.,.F.,.F.)
B_SPLINE_CURVE_WITH_KNOTS((3,2,2,2,2,2,2,2,3),(0.175,0.1775,0.18,0.1825,
0.185,0.1875,0.19,0.1925,0.195),.UNSPECIFIED.)
CURVE()
GEOMETRIC_REPRESENTATION_ITEM()
RATIONAL_B_SPLINE_CURVE((1.,0.923879532511287,1.,0.923879532511287,1.,0.923879532511287,
1.,0.923879532511287,1.,0.923879532511287,1.,0.923879532511287,1.,0.923879532511287,
1.,0.923879532511287,1.))
REPRESENTATION_ITEM('')
);
#753=(
BOUNDED_CURVE()
B_SPLINE_CURVE(2,(#7342,#7343,#7344,#7345,#7346,#7347,#7348,#7349,#7350,
#7351,#7352,#7353,#7354,#7355,#7356,#7357,#7358),.UNSPECIFIED.,.F.,.F.)
B_SPLINE_CURVE_WITH_KNOTS((3,2,2,2,2,2,2,2,3),(0.155,0.1575,0.16,0.1625,
0.165,0.1675,0.17,0.1725,0.175),.UNSPECIFIED.)
CURVE()
GEOMETRIC_REPRESENTATION_ITEM()
RATIONAL_B_SPLINE_CURVE((1.,0.923879532511287,1.,0.923879532511287,1.,0.923879532511287,
1.,0.923879532511287,1.,0.923879532511287,1.,0.923879532511287,1.,0.923879532511287,
1.,0.923879532511287,1.))
REPRESENTATION_ITEM('')
);
#754=(
BOUNDED_CURVE()
B_SPLINE_CURVE(2,(#7363,#7364,#7365,#7366,#7367,#7368,#7369,#7370,#7371,
#7372,#7373,#7374,#7375,#7376,#7377,#7378,#7379),.UNSPECIFIED.,.F.,.F.)
B_SPLINE_CURVE_WITH_KNOTS((3,2,2,2,2,2,2,2,3),(0.155,0.1575,0.16,0.1625,
0.165,0.1675,0.17,0.1725,0.175),.UNSPECIFIED.)
CURVE()
GEOMETRIC_REPRESENTATION_ITEM()
RATIONAL_B_SPLINE_CURVE((1.,0.923879532511287,1.,0.923879532511287,1.,0.923879532511287,
1.,0.923879532511287,1.,0.923879532511287,1.,0.923879532511287,1.,0.923879532511287,
1.,0.923879532511287,1.))
REPRESENTATION_ITEM('')
);
#755=(
BOUNDED_CURVE()
B_SPLINE_CURVE(2,(#7380,#7381,#7382,#7383,#7384,#7385,#7386,#7387,#7388,
#7389,#7390,#7391,#7392,#7393,#7394,#7395,#7396),.UNSPECIFIED.,.F.,.F.)
B_SPLINE_CURVE_WITH_KNOTS((3,2,2,2,2,2,2,2,3),(0.135,0.1375,0.14,0.1425,
0.145,0.1475,0.15,0.1525,0.155),.UNSPECIFIED.)
CURVE()
GEOMETRIC_REPRESENTATION_ITEM()
RATIONAL_B_SPLINE_CURVE((1.,0.923879532511287,1.,0.923879532511287,1.,0.923879532511287,
1.,0.923879532511287,1.,0.923879532511287,1.,0.923879532511287,1.,0.923879532511287,
1.,0.923879532511287,1.))
REPRESENTATION_ITEM('')
);
#756=(
BOUNDED_CURVE()
B_SPLINE_CURVE(2,(#7401,#7402,#7403,#7404,#7405,#7406,#7407,#7408,#7409,
#7410,#7411,#7412,#7413,#7414,#7415,#7416,#7417),.UNSPECIFIED.,.F.,.F.)
B_SPLINE_CURVE_WITH_KNOTS((3,2,2,2,2,2,2,2,3),(0.135,0.1375,0.14,0.1425,
0.145,0.1475,0.15,0.1525,0.155),.UNSPECIFIED.)
CURVE()
GEOMETRIC_REPRESENTATION_ITEM()
RATIONAL_B_SPLINE_CURVE((1.,0.923879532511287,1.,0.923879532511287,1.,0.923879532511287,
1.,0.923879532511287,1.,0.923879532511287,1.,0.923879532511287,1.,0.923879532511287,
1.,0.923879532511287,1.))
REPRESENTATION_ITEM('')
);
#757=(
BOUNDED_CURVE()
B_SPLINE_CURVE(2,(#7418,#7419,#7420,#7421,#7422,#7423,#7424,#7425,#7426,
#7427,#7428,#7429,#7430,#7431,#7432,#7433,#7434),.UNSPECIFIED.,.F.,.F.)
B_SPLINE_CURVE_WITH_KNOTS((3,2,2,2,2,2,2,2,3),(0.115,0.1175,0.12,0.1225,
0.125,0.1275,0.13,0.1325,0.135),.UNSPECIFIED.)
CURVE()
GEOMETRIC_REPRESENTATION_ITEM()
RATIONAL_B_SPLINE_CURVE((1.,0.923879532511287,1.,0.923879532511287,1.,0.923879532511287,
1.,0.923879532511287,1.,0.923879532511287,1.,0.923879532511287,1.,0.923879532511287,
1.,0.923879532511287,1.))
REPRESENTATION_ITEM('')
);
#758=(
BOUNDED_CURVE()
B_SPLINE_CURVE(2,(#7439,#7440,#7441,#7442,#7443,#7444,#7445,#7446,#7447,
#7448,#7449,#7450,#7451,#7452,#7453,#7454,#7455),.UNSPECIFIED.,.F.,.F.)
B_SPLINE_CURVE_WITH_KNOTS((3,2,2,2,2,2,2,2,3),(0.115,0.1175,0.12,0.1225,
0.125,0.1275,0.13,0.1325,0.135),.UNSPECIFIED.)
CURVE()
GEOMETRIC_REPRESENTATION_ITEM()
RATIONAL_B_SPLINE_CURVE((1.,0.923879532511287,1.,0.923879532511287,1.,0.923879532511287,
1.,0.923879532511287,1.,0.923879532511287,1.,0.923879532511287,1.,0.923879532511287,
1.,0.923879532511287,1.))
REPRESENTATION_ITEM('')
);
#759=(
BOUNDED_CURVE()
B_SPLINE_CURVE(2,(#7456,#7457,#7458,#7459,#7460,#7461,#7462,#7463,#7464,
#7465,#7466,#7467,#7468,#7469,#7470,#7471,#7472),.UNSPECIFIED.,.F.,.F.)
B_SPLINE_CURVE_WITH_KNOTS((3,2,2,2,2,2,2,2,3),(0.095,0.0975,0.1,0.1025,
0.105,0.1075,0.11,0.1125,0.115),.UNSPECIFIED.)
CURVE()
GEOMETRIC_REPRESENTATION_ITEM()
RATIONAL_B_SPLINE_CURVE((1.,0.923879532511287,1.,0.923879532511287,1.,0.923879532511287,
1.,0.923879532511287,1.,0.923879532511287,1.,0.923879532511287,1.,0.923879532511287,
1.,0.923879532511287,1.))
REPRESENTATION_ITEM('')
);
#760=(
BOUNDED_CURVE()
B_SPLINE_CURVE(2,(#7477,#7478,#7479,#7480,#7481,#7482,#7483,#7484,#7485,
#7486,#7487,#7488,#7489,#7490,#7491,#7492,#7493),.UNSPECIFIED.,.F.,.F.)
B_SPLINE_CURVE_WITH_KNOTS((3,2,2,2,2,2,2,2,3),(0.095,0.0975,0.1,0.1025,
0.105,0.1075,0.11,0.1125,0.115),.UNSPECIFIED.)
CURVE()
GEOMETRIC_REPRESENTATION_ITEM()
RATIONAL_B_SPLINE_CURVE((1.,0.923879532511287,1.,0.923879532511287,1.,0.923879532511287,
1.,0.923879532511287,1.,0.923879532511287,1.,0.923879532511287,1.,0.923879532511287,
1.,0.923879532511287,1.))
REPRESENTATION_ITEM('')
);
#761=(
BOUNDED_CURVE()
B_SPLINE_CURVE(2,(#7494,#7495,#7496,#7497,#7498,#7499,#7500,#7501,#7502,
#7503,#7504,#7505,#7506,#7507,#7508,#7509,#7510),.UNSPECIFIED.,.F.,.F.)
B_SPLINE_CURVE_WITH_KNOTS((3,2,2,2,2,2,2,2,3),(0.075,0.0775,0.08,0.0825,
0.085,0.0875,0.09,0.0925,0.095),.UNSPECIFIED.)
CURVE()
GEOMETRIC_REPRESENTATION_ITEM()
RATIONAL_B_SPLINE_CURVE((1.,0.923879532511287,1.,0.923879532511287,1.,0.923879532511287,
1.,0.923879532511287,1.,0.923879532511287,1.,0.923879532511287,1.,0.923879532511287,
1.,0.923879532511287,1.))
REPRESENTATION_ITEM('')
);
#762=(
BOUNDED_CURVE()
B_SPLINE_CURVE(2,(#7515,#7516,#7517,#7518,#7519,#7520,#7521,#7522,#7523,
#7524,#7525,#7526,#7527,#7528,#7529,#7530,#7531),.UNSPECIFIED.,.F.,.F.)
B_SPLINE_CURVE_WITH_KNOTS((3,2,2,2,2,2,2,2,3),(0.075,0.0775,0.08,0.0825,
0.085,0.0875,0.09,0.0925,0.095),.UNSPECIFIED.)
CURVE()
GEOMETRIC_REPRESENTATION_ITEM()
RATIONAL_B_SPLINE_CURVE((1.,0.923879532511287,1.,0.923879532511287,1.,0.923879532511287,
1.,0.923879532511287,1.,0.923879532511287,1.,0.923879532511287,1.,0.923879532511287,
1.,0.923879532511287,1.))
REPRESENTATION_ITEM('')
);
#763=(
BOUNDED_CURVE()
B_SPLINE_CURVE(2,(#7532,#7533,#7534,#7535,#7536,#7537,#7538,#7539,#7540,
#7541,#7542,#7543,#7544,#7545,#7546,#7547,#7548),.UNSPECIFIED.,.F.,.F.)
B_SPLINE_CURVE_WITH_KNOTS((3,2,2,2,2,2,2,2,3),(0.055,0.0575,0.06,0.0625,
0.065,0.0675,0.07,0.0725,0.075),.UNSPECIFIED.)
CURVE()
GEOMETRIC_REPRESENTATION_ITEM()
RATIONAL_B_SPLINE_CURVE((1.,0.923879532511287,1.,0.923879532511287,1.,0.923879532511287,
1.,0.923879532511287,1.,0.923879532511287,1.,0.923879532511287,1.,0.923879532511287,
1.,0.923879532511287,1.))
REPRESENTATION_ITEM('')
);
#764=(
BOUNDED_CURVE()
B_SPLINE_CURVE(2,(#7553,#7554,#7555,#7556,#7557,#7558,#7559,#7560,#7561,
#7562,#7563,#7564,#7565,#7566,#7567,#7568,#7569),.UNSPECIFIED.,.F.,.F.)
B_SPLINE_CURVE_WITH_KNOTS((3,2,2,2,2,2,2,2,3),(0.055,0.0575,0.06,0.0625,
0.065,0.0675,0.07,0.0725,0.075),.UNSPECIFIED.)
CURVE()
GEOMETRIC_REPRESENTATION_ITEM()
RATIONAL_B_SPLINE_CURVE((1.,0.923879532511287,1.,0.923879532511287,1.,0.923879532511287,
1.,0.923879532511287,1.,0.923879532511287,1.,0.923879532511287,1.,0.923879532511287,
1.,0.923879532511287,1.))
REPRESENTATION_ITEM('')
);
#765=(
BOUNDED_CURVE()
B_SPLINE_CURVE(2,(#7570,#7571,#7572,#7573,#7574,#7575,#7576,#7577,#7578,
#7579,#7580,#7581,#7582,#7583,#7584,#7585,#7586),.UNSPECIFIED.,.F.,.F.)
B_SPLINE_CURVE_WITH_KNOTS((3,2,2,2,2,2,2,2,3),(0.035,0.0375,0.04,0.0425,
0.045,0.0475,0.05,0.0525,0.055),.UNSPECIFIED.)
CURVE()
GEOMETRIC_REPRESENTATION_ITEM()
RATIONAL_B_SPLINE_CURVE((1.,0.923879532511287,1.,0.923879532511287,1.,0.923879532511287,
1.,0.923879532511287,1.,0.923879532511287,1.,0.923879532511287,1.,0.923879532511287,
1.,0.923879532511287,1.))
REPRESENTATION_ITEM('')
);
#766=(
BOUNDED_CURVE()
B_SPLINE_CURVE(2,(#7593,#7594,#7595,#7596,#7597,#7598,#7599,#7600,#7601,
#7602,#7603,#7604,#7605,#7606,#7607,#7608,#7609),.UNSPECIFIED.,.F.,.F.)
B_SPLINE_CURVE_WITH_KNOTS((3,2,2,2,2,2,2,2,3),(0.015,0.0175,0.02,0.0225,
0.025,0.0275,0.03,0.0325,0.035),.UNSPECIFIED.)
CURVE()
GEOMETRIC_REPRESENTATION_ITEM()
RATIONAL_B_SPLINE_CURVE((1.,0.923879532511287,1.,0.923879532511287,1.,0.923879532511287,
1.,0.923879532511287,1.,0.923879532511287,1.,0.923879532511287,1.,0.923879532511287,
1.,0.923879532511287,1.))
REPRESENTATION_ITEM('')
);
#767=(
BOUNDED_CURVE()
B_SPLINE_CURVE(2,(#7613,#7614,#7615,#7616,#7617,#7618,#7619,#7620,#7621,
#7622,#7623,#7624,#7625),.UNSPECIFIED.,.F.,.F.)
B_SPLINE_CURVE_WITH_KNOTS((3,2,2,2,2,2,3),(0.,0.0025,0.005,0.0075,0.01,
0.0125,0.015),.UNSPECIFIED.)
CURVE()
GEOMETRIC_REPRESENTATION_ITEM()
RATIONAL_B_SPLINE_CURVE((1.,0.923879532511287,1.,0.923879532511287,1.,0.923879532511287,
1.,0.923879532511287,1.,0.923879532511287,1.,0.923879532511287,1.))
REPRESENTATION_ITEM('')
);
#768=(
BOUNDED_CURVE()
B_SPLINE_CURVE(2,(#7628,#7629,#7630,#7631,#7632,#7633,#7634,#7635,#7636,
#7637,#7638,#7639,#7640),.UNSPECIFIED.,.F.,.F.)
B_SPLINE_CURVE_WITH_KNOTS((3,2,2,2,2,2,3),(0.,0.0025,0.005,0.0075,0.01,
0.0125,0.015),.UNSPECIFIED.)
CURVE()
GEOMETRIC_REPRESENTATION_ITEM()
RATIONAL_B_SPLINE_CURVE((1.,0.923879532511287,1.,0.923879532511287,1.,0.923879532511287,
1.,0.923879532511287,1.,0.923879532511287,1.,0.923879532511287,1.))
REPRESENTATION_ITEM('')
);
#769=(
BOUNDED_CURVE()
B_SPLINE_CURVE(2,(#7726,#7727,#7728,#7729,#7730,#7731,#7732,#7733,#7734,
#7735,#7736,#7737,#7738,#7739,#7740,#7741,#7742),.UNSPECIFIED.,.F.,.F.)
B_SPLINE_CURVE_WITH_KNOTS((3,2,2,2,2,2,2,2,3),(0.035,0.0375,0.04,0.0425,
0.045,0.0475,0.05,0.0525,0.055),.UNSPECIFIED.)
CURVE()
GEOMETRIC_REPRESENTATION_ITEM()
RATIONAL_B_SPLINE_CURVE((1.,0.923879532511287,1.,0.923879532511287,1.,0.923879532511287,
1.,0.923879532511287,1.,0.923879532511287,1.,0.923879532511287,1.,0.923879532511287,
1.,0.923879532511287,1.))
REPRESENTATION_ITEM('')
);
#770=(
BOUNDED_CURVE()
B_SPLINE_CURVE(2,(#7743,#7744,#7745,#7746,#7747,#7748,#7749,#7750,#7751,
#7752,#7753,#7754,#7755,#7756,#7757,#7758,#7759),.UNSPECIFIED.,.F.,.F.)
B_SPLINE_CURVE_WITH_KNOTS((3,2,2,2,2,2,2,2,3),(0.015,0.0175,0.02,0.0225,
0.025,0.0275,0.03,0.0325,0.035),.UNSPECIFIED.)
CURVE()
GEOMETRIC_REPRESENTATION_ITEM()
RATIONAL_B_SPLINE_CURVE((1.,0.923879532511287,1.,0.923879532511287,1.,0.923879532511287,
1.,0.923879532511287,1.,0.923879532511287,1.,0.923879532511287,1.,0.923879532511287,
1.,0.923879532511287,1.))
REPRESENTATION_ITEM('')
);
#771=(
BOUNDED_CURVE()
B_SPLINE_CURVE(2,(#9384,#9385,#9386,#9387,#9388,#9389,#9390,#9391,#9392,
#9393,#9394,#9395,#9396,#9397,#9398,#9399,#9400),.UNSPECIFIED.,.F.,.F.)
B_SPLINE_CURVE_WITH_KNOTS((3,2,2,2,2,2,2,2,3),(0.01,0.0125,0.015,0.0175,
0.02,0.0225,0.025,0.0275,0.03),.UNSPECIFIED.)
CURVE()
GEOMETRIC_REPRESENTATION_ITEM()
RATIONAL_B_SPLINE_CURVE((1.,0.923879532511287,1.,0.923879532511287,1.,0.923879532511287,
1.,0.923879532511287,1.,0.923879532511287,1.,0.923879532511287,1.,0.923879532511287,
1.,0.923879532511287,1.))
REPRESENTATION_ITEM('')
);
#772=(
BOUNDED_CURVE()
B_SPLINE_CURVE(2,(#9402,#9403,#9404,#9405,#9406,#9407,#9408,#9409,#9410,
#9411,#9412,#9413,#9414,#9415,#9416,#9417,#9418),.UNSPECIFIED.,.F.,.F.)
B_SPLINE_CURVE_WITH_KNOTS((3,2,2,2,2,2,2,2,3),(0.01,0.0125,0.015,0.0175,
0.02,0.0225,0.025,0.0275,0.03),.UNSPECIFIED.)
CURVE()
GEOMETRIC_REPRESENTATION_ITEM()
RATIONAL_B_SPLINE_CURVE((1.,0.923879532511287,1.,0.923879532511287,1.,0.923879532511287,
1.,0.923879532511287,1.,0.923879532511287,1.,0.923879532511287,1.,0.923879532511287,
1.,0.923879532511287,1.))
REPRESENTATION_ITEM('')
);
#773=(
BOUNDED_CURVE()
B_SPLINE_CURVE(2,(#11021,#11022,#11023,#11024,#11025,#11026,#11027,#11028,
#11029,#11030,#11031,#11032,#11033,#11034,#11035),.UNSPECIFIED.,.F.,.F.)
B_SPLINE_CURVE_WITH_KNOTS((3,2,2,2,2,2,2,3),(0.9825,0.985,0.9875,0.99,0.9925,
0.995,0.9975,1.),.UNSPECIFIED.)
CURVE()
GEOMETRIC_REPRESENTATION_ITEM()
RATIONAL_B_SPLINE_CURVE((1.,0.923879532511287,1.,0.923879532511287,1.,0.923879532511287,
1.,0.923879532511287,1.,0.923879532511287,1.,0.923879532511287,1.,0.923879532511287,
1.))
REPRESENTATION_ITEM('')
);
#774=(
BOUNDED_CURVE()
B_SPLINE_CURVE(2,(#11323,#11324,#11325,#11326,#11327,#11328,#11329,#11330,
#11331,#11332,#11333,#11334,#11335,#11336,#11337,#11338,#11339,#11340,#11341,
#11342,#11343,#11344,#11345,#11346,#11347,#11348,#11349,#11350,#11351,#11352,
#11353,#11354,#11355,#11356,#11357,#11358,#11359,#11360,#11361,#11362,#11363,
#11364,#11365),.UNSPECIFIED.,.F.,.F.)
B_SPLINE_CURVE_WITH_KNOTS((3,2,2,2,2,2,2,2,2,2,2,2,2,2,2,2,2,2,2,2,2,3),
(1.82334519084262E-6,0.0166666666666667,0.0333333333333333,0.05,0.0666666666666667,
0.0833333333333333,0.1,0.116666666666667,0.133333333333333,0.15,0.166666666666667,
0.183333333333333,0.2,0.216666666666667,0.233333333333333,0.25,0.266666666666667,
0.283333333333333,0.3,0.316666666666667,0.333333333333333,0.333335156678524),
 .UNSPECIFIED.)
CURVE()
GEOMETRIC_REPRESENTATION_ITEM()
RATIONAL_B_SPLINE_CURVE((0.999997306486108,0.987689687499436,1.,0.987688340595138,
1.,0.987688340595138,1.,0.987688340595138,1.,0.987688340595138,1.,0.987688340595138,
1.,0.987688340595138,1.,0.987688340595138,1.,0.987688340595138,1.,0.987688340595138,
1.,0.987688340595138,1.,0.987688340595138,1.,0.987688340595138,1.,0.987688340595138,
1.,0.987688340595138,1.,0.987688340595138,1.,0.987688340595138,1.,0.987688340595138,
1.,0.987688340595138,1.,0.987688340595138,1.,0.999998653095702,0.999997306486109))
REPRESENTATION_ITEM('')
);
#775=(
BOUNDED_CURVE()
B_SPLINE_CURVE(2,(#11370,#11371,#11372),.UNSPECIFIED.,.F.,.F.)
B_SPLINE_CURVE_WITH_KNOTS((3,3),(0.,1.82334519084262E-6),.UNSPECIFIED.)
CURVE()
GEOMETRIC_REPRESENTATION_ITEM()
RATIONAL_B_SPLINE_CURVE((1.,0.999998653095702,0.999997306486108))
REPRESENTATION_ITEM('')
);
#776=(
BOUNDED_CURVE()
B_SPLINE_CURVE(2,(#11746,#11747,#11748,#11749,#11750,#11751,#11752,#11753,
#11754,#11755,#11756,#11757,#11758,#11759,#11760,#11761,#11762,#11763,#11764,
#11765,#11766,#11767,#11768,#11769,#11770,#11771,#11772,#11773,#11774,#11775,
#11776,#11777,#11778,#11779,#11780,#11781,#11782,#11783,#11784,#11785,#11786),
 .UNSPECIFIED.,.F.,.F.)
B_SPLINE_CURVE_WITH_KNOTS((3,2,2,2,2,2,2,2,2,2,2,2,2,2,2,2,2,2,2,2,3),(0.666668490011857,
0.683333333333333,0.7,0.716666666666667,0.733333333333333,0.75,0.766666666666667,
0.783333333333333,0.8,0.816666666666667,0.833333333333333,0.85,0.866666666666667,
0.883333333333333,0.9,0.916666666666667,0.933333333333333,0.95,0.966666666666667,
0.983333333333333,1.),.UNSPECIFIED.)
CURVE()
GEOMETRIC_REPRESENTATION_ITEM()
RATIONAL_B_SPLINE_CURVE((0.999997306486109,0.987689687499436,1.,0.987688340595138,
1.,0.987688340595138,1.,0.987688340595138,1.,0.987688340595138,1.,0.987688340595138,
1.,0.987688340595138,1.,0.987688340595138,1.,0.987688340595138,1.,0.987688340595138,
1.,0.987688340595138,1.,0.987688340595138,1.,0.987688340595138,1.,0.987688340595138,
1.,0.987688340595138,1.,0.987688340595138,1.,0.987688340595138,1.,0.987688340595138,
1.,0.987688340595138,1.,0.987688340595138,1.))
REPRESENTATION_ITEM('')
);
#777=(
BOUNDED_CURVE()
B_SPLINE_CURVE(2,(#12151,#12152,#12153,#12154,#12155,#12156,#12157,#12158,
#12159,#12160,#12161,#12162,#12163,#12164,#12165,#12166,#12167,#12168,#12169,
#12170,#12171,#12172,#12173,#12174,#12175,#12176,#12177,#12178,#12179,#12180,
#12181,#12182,#12183,#12184,#12185,#12186,#12187,#12188,#12189,#12190,#12191,
#12192,#12193),.UNSPECIFIED.,.F.,.F.)
B_SPLINE_CURVE_WITH_KNOTS((3,2,2,2,2,2,2,2,2,2,2,2,2,2,2,2,2,2,2,2,2,3),
(0.333335156678524,0.35,0.366666666666667,0.383333333333333,0.4,0.416666666666667,
0.433333333333333,0.45,0.466666666666667,0.483333333333333,0.5,0.516666666666667,
0.533333333333333,0.55,0.566666666666667,0.583333333333333,0.6,0.616666666666667,
0.633333333333333,0.65,0.666666666666667,0.666668490011857),
 .UNSPECIFIED.)
CURVE()
GEOMETRIC_REPRESENTATION_ITEM()
RATIONAL_B_SPLINE_CURVE((0.999997306486109,0.987689687499436,1.,0.987688340595138,
1.,0.987688340595138,1.,0.987688340595138,1.,0.987688340595138,1.,0.987688340595138,
1.,0.987688340595138,1.,0.987688340595138,1.,0.987688340595138,1.,0.987688340595138,
1.,0.987688340595138,1.,0.987688340595138,1.,0.987688340595138,1.,0.987688340595138,
1.,0.987688340595138,1.,0.987688340595138,1.,0.987688340595138,1.,0.987688340595138,
1.,0.987688340595138,1.,0.987688340595138,1.,0.999998653095702,0.999997306486109))
REPRESENTATION_ITEM('')
);
#778=(
BOUNDED_CURVE()
B_SPLINE_CURVE(2,(#12820,#12821,#12822,#12823,#12824,#12825,#12826,#12827,
#12828,#12829,#12830,#12831,#12832,#12833,#12834,#12835,#12836,#12837,#12838,
#12839,#12840,#12841,#12842,#12843,#12844,#12845,#12846,#12847,#12848,#12849,
#12850,#12851,#12852,#12853,#12854,#12855,#12856,#12857,#12858,#12859,#12860,
#12861,#12862,#12863,#12864,#12865,#12866,#12867,#12868,#12869,#12870,#12871,
#12872,#12873,#12874,#12875,#12876,#12877,#12878,#12879,#12880,#12881,#12882,
#12883,#12884,#12885,#12886,#12887,#12888,#12889,#12890,#12891,#12892,#12893,
#12894,#12895,#12896,#12897,#12898,#12899,#12900,#12901,#12902,#12903,#12904,
#12905,#12906,#12907,#12908,#12909,#12910,#12911,#12912,#12913,#12914,#12915,
#12916,#12917,#12918,#12919,#12920,#12921,#12922,#12923,#12924,#12925,#12926,
#12927,#12928,#12929,#12930,#12931,#12932,#12933,#12934,#12935,#12936,#12937,
#12938,#12939,#12940),.UNSPECIFIED.,.F.,.F.)
B_SPLINE_CURVE_WITH_KNOTS((3,2,2,2,2,2,2,2,2,2,2,2,2,2,2,2,2,2,2,2,2,2,
2,2,2,2,2,2,2,2,2,2,2,2,2,2,2,2,2,2,2,2,2,2,2,2,2,2,2,2,2,2,2,2,2,2,2,2,
2,2,3),(0.,0.0166666666666667,0.0333333333333333,0.05,0.0666666666666667,
0.0833333333333333,0.1,0.116666666666667,0.133333333333333,0.15,0.166666666666667,
0.183333333333333,0.2,0.216666666666667,0.233333333333333,0.25,0.266666666666667,
0.283333333333333,0.3,0.316666666666667,0.333333333333333,0.35,0.366666666666667,
0.383333333333333,0.4,0.416666666666667,0.433333333333333,0.45,0.466666666666667,
0.483333333333333,0.5,0.516666666666667,0.533333333333333,0.55,0.566666666666667,
0.583333333333333,0.6,0.616666666666667,0.633333333333333,0.65,0.666666666666667,
0.683333333333333,0.7,0.716666666666667,0.733333333333333,0.75,0.766666666666667,
0.783333333333333,0.8,0.816666666666667,0.833333333333333,0.85,0.866666666666667,
0.883333333333333,0.9,0.916666666666667,0.933333333333333,0.95,0.966666666666667,
0.983333333333333,1.),.UNSPECIFIED.)
CURVE()
GEOMETRIC_REPRESENTATION_ITEM()
RATIONAL_B_SPLINE_CURVE((1.,0.987688340595138,1.,0.987688340595138,1.,0.987688340595138,
1.,0.987688340595138,1.,0.987688340595138,1.,0.987688340595138,1.,0.987688340595138,
1.,0.987688340595138,1.,0.987688340595138,1.,0.987688340595138,1.,0.987688340595138,
1.,0.987688340595138,1.,0.987688340595138,1.,0.987688340595138,1.,0.987688340595138,
1.,0.987688340595138,1.,0.987688340595138,1.,0.987688340595138,1.,0.987688340595138,
1.,0.987688340595138,1.,0.987688340595138,1.,0.987688340595138,1.,0.987688340595138,
1.,0.987688340595138,1.,0.987688340595138,1.,0.987688340595138,1.,0.987688340595138,
1.,0.987688340595138,1.,0.987688340595138,1.,0.987688340595138,1.,0.987688340595138,
1.,0.987688340595138,1.,0.987688340595138,1.,0.987688340595138,1.,0.987688340595138,
1.,0.987688340595138,1.,0.987688340595138,1.,0.987688340595138,1.,0.987688340595138,
1.,0.987688340595138,1.,0.987688340595138,1.,0.987688340595138,1.,0.987688340595138,
1.,0.987688340595138,1.,0.987688340595138,1.,0.987688340595138,1.,0.987688340595138,
1.,0.987688340595138,1.,0.987688340595138,1.,0.987688340595138,1.,0.987688340595138,
1.,0.987688340595138,1.,0.987688340595138,1.,0.987688340595138,1.,0.987688340595138,
1.,0.987688340595138,1.,0.987688340595138,1.,0.987688340595138,1.,0.987688340595138,
1.,0.987688340595138,1.))
REPRESENTATION_ITEM('')
);
#779=(
BOUNDED_CURVE()
B_SPLINE_CURVE(2,(#13183,#13184,#13185,#13186,#13187,#13188,#13189,#13190,
#13191,#13192,#13193,#13194,#13195,#13196,#13197,#13198,#13199,#13200,#13201,
#13202,#13203,#13204,#13205,#13206,#13207,#13208,#13209,#13210,#13211,#13212,
#13213,#13214,#13215,#13216,#13217,#13218,#13219,#13220,#13221,#13222,#13223,
#13224,#13225,#13226,#13227,#13228,#13229,#13230,#13231,#13232,#13233,#13234,
#13235,#13236,#13237,#13238,#13239,#13240,#13241,#13242,#13243,#13244,#13245,
#13246,#13247,#13248,#13249,#13250,#13251,#13252,#13253,#13254,#13255,#13256,
#13257,#13258,#13259,#13260,#13261,#13262,#13263,#13264,#13265,#13266,#13267,
#13268,#13269,#13270,#13271,#13272,#13273,#13274,#13275,#13276,#13277,#13278,
#13279,#13280,#13281,#13282,#13283,#13284,#13285,#13286,#13287,#13288,#13289,
#13290,#13291,#13292,#13293,#13294,#13295,#13296,#13297,#13298,#13299,#13300,
#13301,#13302,#13303),.UNSPECIFIED.,.F.,.F.)
B_SPLINE_CURVE_WITH_KNOTS((3,2,2,2,2,2,2,2,2,2,2,2,2,2,2,2,2,2,2,2,2,2,
2,2,2,2,2,2,2,2,2,2,2,2,2,2,2,2,2,2,2,2,2,2,2,2,2,2,2,2,2,2,2,2,2,2,2,2,
2,2,3),(0.,0.0166666666666667,0.0333333333333333,0.05,0.0666666666666667,
0.0833333333333333,0.1,0.116666666666667,0.133333333333333,0.15,0.166666666666667,
0.183333333333333,0.2,0.216666666666667,0.233333333333333,0.25,0.266666666666667,
0.283333333333333,0.3,0.316666666666667,0.333333333333333,0.35,0.366666666666667,
0.383333333333333,0.4,0.416666666666667,0.433333333333333,0.45,0.466666666666667,
0.483333333333333,0.5,0.516666666666667,0.533333333333333,0.55,0.566666666666667,
0.583333333333333,0.6,0.616666666666667,0.633333333333333,0.65,0.666666666666667,
0.683333333333333,0.7,0.716666666666667,0.733333333333333,0.75,0.766666666666667,
0.783333333333333,0.8,0.816666666666667,0.833333333333333,0.85,0.866666666666667,
0.883333333333333,0.9,0.916666666666667,0.933333333333333,0.95,0.966666666666667,
0.983333333333333,1.),.UNSPECIFIED.)
CURVE()
GEOMETRIC_REPRESENTATION_ITEM()
RATIONAL_B_SPLINE_CURVE((1.,0.987688340595138,1.,0.987688340595138,1.,0.987688340595138,
1.,0.987688340595138,1.,0.987688340595138,1.,0.987688340595138,1.,0.987688340595138,
1.,0.987688340595138,1.,0.987688340595138,1.,0.987688340595138,1.,0.987688340595138,
1.,0.987688340595138,1.,0.987688340595138,1.,0.987688340595138,1.,0.987688340595138,
1.,0.987688340595138,1.,0.987688340595138,1.,0.987688340595138,1.,0.987688340595138,
1.,0.987688340595138,1.,0.987688340595138,1.,0.987688340595138,1.,0.987688340595138,
1.,0.987688340595138,1.,0.987688340595138,1.,0.987688340595138,1.,0.987688340595138,
1.,0.987688340595138,1.,0.987688340595138,1.,0.987688340595138,1.,0.987688340595138,
1.,0.987688340595138,1.,0.987688340595138,1.,0.987688340595138,1.,0.987688340595138,
1.,0.987688340595138,1.,0.987688340595138,1.,0.987688340595138,1.,0.987688340595138,
1.,0.987688340595138,1.,0.987688340595138,1.,0.987688340595138,1.,0.987688340595138,
1.,0.987688340595138,1.,0.987688340595138,1.,0.987688340595138,1.,0.987688340595138,
1.,0.987688340595138,1.,0.987688340595138,1.,0.987688340595138,1.,0.987688340595138,
1.,0.987688340595138,1.,0.987688340595138,1.,0.987688340595138,1.,0.987688340595138,
1.,0.987688340595138,1.,0.987688340595138,1.,0.987688340595138,1.,0.987688340595138,
1.,0.987688340595138,1.))
REPRESENTATION_ITEM('')
);
#780=LINE('',#3911,#931);
#781=LINE('',#3923,#932);
#782=LINE('',#3936,#933);
#783=LINE('',#3974,#934);
#784=LINE('',#4012,#935);
#785=LINE('',#4050,#936);
#786=LINE('',#4088,#937);
#787=LINE('',#4126,#938);
#788=LINE('',#4164,#939);
#789=LINE('',#4202,#940);
#790=LINE('',#4240,#941);
#791=LINE('',#4278,#942);
#792=LINE('',#4316,#943);
#793=LINE('',#4354,#944);
#794=LINE('',#4392,#945);
#795=LINE('',#4430,#946);
#796=LINE('',#4468,#947);
#797=LINE('',#4506,#948);
#798=LINE('',#4544,#949);
#799=LINE('',#4582,#950);
#800=LINE('',#4620,#951);
#801=LINE('',#4658,#952);
#802=LINE('',#4696,#953);
#803=LINE('',#4734,#954);
#804=LINE('',#4772,#955);
#805=LINE('',#4810,#956);
#806=LINE('',#4848,#957);
#807=LINE('',#4886,#958);
#808=LINE('',#4924,#959);
#809=LINE('',#4962,#960);
#810=LINE('',#5000,#961);
#811=LINE('',#5038,#962);
#812=LINE('',#5076,#963);
#813=LINE('',#5114,#964);
#814=LINE('',#5152,#965);
#815=LINE('',#5190,#966);
#816=LINE('',#5228,#967);
#817=LINE('',#5266,#968);
#818=LINE('',#5304,#969);
#819=LINE('',#5342,#970);
#820=LINE('',#5380,#971);
#821=LINE('',#5418,#972);
#822=LINE('',#5456,#973);
#823=LINE('',#5494,#974);
#824=LINE('',#5532,#975);
#825=LINE('',#5570,#976);
#826=LINE('',#5608,#977);
#827=LINE('',#5646,#978);
#828=LINE('',#5684,#979);
#829=LINE('',#5722,#980);
#830=LINE('',#5760,#981);
#831=LINE('',#5772,#982);
#832=LINE('',#5785,#983);
#833=LINE('',#5804,#984);
#834=LINE('',#5842,#985);
#835=LINE('',#5880,#986);
#836=LINE('',#5918,#987);
#837=LINE('',#5956,#988);
#838=LINE('',#5994,#989);
#839=LINE('',#6032,#990);
#840=LINE('',#6070,#991);
#841=LINE('',#6108,#992);
#842=LINE('',#6146,#993);
#843=LINE('',#6184,#994);
#844=LINE('',#6222,#995);
#845=LINE('',#6260,#996);
#846=LINE('',#6298,#997);
#847=LINE('',#6336,#998);
#848=LINE('',#6374,#999);
#849=LINE('',#6412,#1000);
#850=LINE('',#6450,#1001);
#851=LINE('',#6488,#1002);
#852=LINE('',#6526,#1003);
#853=LINE('',#6564,#1004);
#854=LINE('',#6602,#1005);
#855=LINE('',#6640,#1006);
#856=LINE('',#6678,#1007);
#857=LINE('',#6716,#1008);
#858=LINE('',#6754,#1009);
#859=LINE('',#6792,#1010);
#860=LINE('',#6830,#1011);
#861=LINE('',#6868,#1012);
#862=LINE('',#6906,#1013);
#863=LINE('',#6944,#1014);
#864=LINE('',#6982,#1015);
#865=LINE('',#7020,#1016);
#866=LINE('',#7058,#1017);
#867=LINE('',#7096,#1018);
#868=LINE('',#7134,#1019);
#869=LINE('',#7172,#1020);
#870=LINE('',#7210,#1021);
#871=LINE('',#7248,#1022);
#872=LINE('',#7286,#1023);
#873=LINE('',#7324,#1024);
#874=LINE('',#7362,#1025);
#875=LINE('',#7400,#1026);
#876=LINE('',#7438,#1027);
#877=LINE('',#7476,#1028);
#878=LINE('',#7514,#1029);
#879=LINE('',#7552,#1030);
#880=LINE('',#7591,#1031);
#881=LINE('',#7611,#1032);
#882=LINE('',#7627,#1033);
#883=LINE('',#7647,#1034);
#884=LINE('',#7773,#1035);
#885=LINE('',#7775,#1036);
#886=LINE('',#7776,#1037);
#887=LINE('',#7778,#1038);
#888=LINE('',#7780,#1039);
#889=LINE('',#7781,#1040);
#890=LINE('',#11039,#1041);
#891=LINE('',#11044,#1042);
#892=LINE('',#11048,#1043);
#893=LINE('',#11050,#1044);
#894=LINE('',#11059,#1045);
#895=LINE('',#11067,#1046);
#896=LINE('',#11070,#1047);
#897=LINE('',#11139,#1048);
#898=LINE('',#11152,#1049);
#899=LINE('',#11216,#1050);
#900=LINE('',#11220,#1051);
#901=LINE('',#11227,#1052);
#902=LINE('',#11233,#1053);
#903=LINE('',#11244,#1054);
#904=LINE('',#11249,#1055);
#905=LINE('',#11253,#1056);
#906=LINE('',#11258,#1057);
#907=LINE('',#11265,#1058);
#908=LINE('',#11284,#1059);
#909=LINE('',#11293,#1060);
#910=LINE('',#11302,#1061);
#911=LINE('',#11308,#1062);
#912=LINE('',#11315,#1063);
#913=LINE('',#11321,#1064);
#914=LINE('',#11367,#1065);
#915=LINE('',#11383,#1066);
#916=LINE('',#11788,#1067);
#917=LINE('',#12565,#1068);
#918=LINE('',#12566,#1069);
#919=LINE('',#12576,#1070);
#920=LINE('',#12577,#1071);
#921=LINE('',#13551,#1072);
#922=LINE('',#13554,#1073);
#923=LINE('',#13557,#1074);
#924=LINE('',#13559,#1075);
#925=LINE('',#13560,#1076);
#926=LINE('',#13563,#1077);
#927=LINE('',#13565,#1078);
#928=LINE('',#13566,#1079);
#929=LINE('',#13568,#1080);
#930=LINE('',#13569,#1081);
#931=VECTOR('',#3284,104.958734125);
#932=VECTOR('',#3285,0.25);
#933=VECTOR('',#3288,104.958734125);
#934=VECTOR('',#3291,104.958734125);
#935=VECTOR('',#3294,104.958734125);
#936=VECTOR('',#3297,104.958734125);
#937=VECTOR('',#3300,104.958734125);
#938=VECTOR('',#3303,104.958734125);
#939=VECTOR('',#3306,104.958734125);
#940=VECTOR('',#3309,104.958734125);
#941=VECTOR('',#3312,104.958734125);
#942=VECTOR('',#3315,104.958734125);
#943=VECTOR('',#3318,104.958734125);
#944=VECTOR('',#3321,104.958734125);
#945=VECTOR('',#3324,104.958734125);
#946=VECTOR('',#3327,104.958734125);
#947=VECTOR('',#3330,104.958734125);
#948=VECTOR('',#3333,104.958734125);
#949=VECTOR('',#3336,104.958734125);
#950=VECTOR('',#3339,104.958734125);
#951=VECTOR('',#3342,104.958734125);
#952=VECTOR('',#3345,104.958734125);
#953=VECTOR('',#3348,104.958734125);
#954=VECTOR('',#3351,104.958734125);
#955=VECTOR('',#3354,104.958734125);
#956=VECTOR('',#3357,104.958734125);
#957=VECTOR('',#3360,104.958734125);
#958=VECTOR('',#3363,104.958734125);
#959=VECTOR('',#3366,104.958734125);
#960=VECTOR('',#3369,104.958734125);
#961=VECTOR('',#3372,104.958734125);
#962=VECTOR('',#3375,104.958734125);
#963=VECTOR('',#3378,104.958734125);
#964=VECTOR('',#3381,104.958734125);
#965=VECTOR('',#3384,104.958734125);
#966=VECTOR('',#3387,104.958734125);
#967=VECTOR('',#3390,104.958734125);
#968=VECTOR('',#3393,104.958734125);
#969=VECTOR('',#3396,104.958734125);
#970=VECTOR('',#3399,104.958734125);
#971=VECTOR('',#3402,104.958734125);
#972=VECTOR('',#3405,104.958734125);
#973=VECTOR('',#3408,104.958734125);
#974=VECTOR('',#3411,104.958734125);
#975=VECTOR('',#3414,104.958734125);
#976=VECTOR('',#3417,104.958734125);
#977=VECTOR('',#3420,104.958734125);
#978=VECTOR('',#3423,104.958734125);
#979=VECTOR('',#3426,104.958734125);
#980=VECTOR('',#3429,104.958734125);
#981=VECTOR('',#3432,104.958734125);
#982=VECTOR('',#3433,0.250000000000004);
#983=VECTOR('',#3436,105.5);
#984=VECTOR('',#3441,105.5);
#985=VECTOR('',#3444,105.5);
#986=VECTOR('',#3447,105.5);
#987=VECTOR('',#3450,105.5);
#988=VECTOR('',#3453,105.5);
#989=VECTOR('',#3456,105.5);
#990=VECTOR('',#3459,105.5);
#991=VECTOR('',#3462,105.5);
#992=VECTOR('',#3465,105.5);
#993=VECTOR('',#3468,105.5);
#994=VECTOR('',#3471,105.5);
#995=VECTOR('',#3474,105.5);
#996=VECTOR('',#3477,105.5);
#997=VECTOR('',#3480,105.5);
#998=VECTOR('',#3483,105.5);
#999=VECTOR('',#3486,105.5);
#1000=VECTOR('',#3489,105.5);
#1001=VECTOR('',#3492,105.5);
#1002=VECTOR('',#3495,105.5);
#1003=VECTOR('',#3498,105.5);
#1004=VECTOR('',#3501,105.5);
#1005=VECTOR('',#3504,105.5);
#1006=VECTOR('',#3507,105.5);
#1007=VECTOR('',#3510,105.5);
#1008=VECTOR('',#3513,105.5);
#1009=VECTOR('',#3516,105.5);
#1010=VECTOR('',#3519,105.5);
#1011=VECTOR('',#3522,105.5);
#1012=VECTOR('',#3525,105.5);
#1013=VECTOR('',#3528,105.5);
#1014=VECTOR('',#3531,105.5);
#1015=VECTOR('',#3534,105.5);
#1016=VECTOR('',#3537,105.5);
#1017=VECTOR('',#3540,105.5);
#1018=VECTOR('',#3543,105.5);
#1019=VECTOR('',#3546,105.5);
#1020=VECTOR('',#3549,105.5);
#1021=VECTOR('',#3552,105.5);
#1022=VECTOR('',#3555,105.5);
#1023=VECTOR('',#3558,105.5);
#1024=VECTOR('',#3561,105.5);
#1025=VECTOR('',#3564,105.5);
#1026=VECTOR('',#3567,105.5);
#1027=VECTOR('',#3570,105.5);
#1028=VECTOR('',#3573,105.5);
#1029=VECTOR('',#3576,105.5);
#1030=VECTOR('',#3579,105.5);
#1031=VECTOR('',#3584,105.5);
#1032=VECTOR('',#3585,105.5);
#1033=VECTOR('',#3586,0.874999997268811);
#1034=VECTOR('',#3593,120.5);
#1035=VECTOR('',#3616,118.168461709225);
#1036=VECTOR('',#3619,0.624999997268823);
#1037=VECTOR('',#3620,0.624999997268819);
#1038=VECTOR('',#3623,0.624999997268823);
#1039=VECTOR('',#3624,0.624999997268822);
#1040=VECTOR('',#3625,0.874999997268824);
#1041=VECTOR('',#3632,9.99999999999999);
#1042=VECTOR('',#3639,9.99999999999999);
#1043=VECTOR('',#3646,114.797295826488);
#1044=VECTOR('',#3649,120.5);
#1045=VECTOR('',#3660,15.);
#1046=VECTOR('',#3671,9.99999999999999);
#1047=VECTOR('',#3676,15.);
#1048=VECTOR('',#3687,12.5);
#1049=VECTOR('',#3704,15.);
#1050=VECTOR('',#3707,14.);
#1051=VECTOR('',#3712,13.5);
#1052=VECTOR('',#3721,12.5);
#1053=VECTOR('',#3728,11.5);
#1054=VECTOR('',#3743,52.);
#1055=VECTOR('',#3750,200.);
#1056=VECTOR('',#3755,50.);
#1057=VECTOR('',#3760,52.);
#1058=VECTOR('',#3769,56.);
#1059=VECTOR('',#3796,15.);
#1060=VECTOR('',#3807,14.);
#1061=VECTOR('',#3818,12.5);
#1062=VECTOR('',#3825,11.5);
#1063=VECTOR('',#3836,11.);
#1064=VECTOR('',#3843,7.5);
#1065=VECTOR('',#3844,7.5);
#1066=VECTOR('',#3853,7.5);
#1067=VECTOR('',#3856,7.5);
#1068=VECTOR('',#3863,42.5163970020424);
#1069=VECTOR('',#3864,3.);
#1070=VECTOR('',#3867,3.);
#1071=VECTOR('',#3868,42.5163970020424);
#1072=VECTOR('',#3873,50.);
#1073=VECTOR('',#3876,50.);
#1074=VECTOR('',#3879,8.50510257216822);
#1075=VECTOR('',#3880,50.);
#1076=VECTOR('',#3881,8.50510257216822);
#1077=VECTOR('',#3884,10.);
#1078=VECTOR('',#3885,50.);
#1079=VECTOR('',#3886,10.);
#1080=VECTOR('',#3889,8.50510257216822);
#1081=VECTOR('',#3890,8.50510257216822);
#1082=VERTEX_POINT('',#3909);
#1083=VERTEX_POINT('',#3910);
#1084=VERTEX_POINT('',#3912);
#1085=VERTEX_POINT('',#3922);
#1086=VERTEX_POINT('',#3934);
#1087=VERTEX_POINT('',#3935);
#1088=VERTEX_POINT('',#3972);
#1089=VERTEX_POINT('',#3973);
#1090=VERTEX_POINT('',#4010);
#1091=VERTEX_POINT('',#4011);
#1092=VERTEX_POINT('',#4048);
#1093=VERTEX_POINT('',#4049);
#1094=VERTEX_POINT('',#4086);
#1095=VERTEX_POINT('',#4087);
#1096=VERTEX_POINT('',#4124);
#1097=VERTEX_POINT('',#4125);
#1098=VERTEX_POINT('',#4162);
#1099=VERTEX_POINT('',#4163);
#1100=VERTEX_POINT('',#4200);
#1101=VERTEX_POINT('',#4201);
#1102=VERTEX_POINT('',#4238);
#1103=VERTEX_POINT('',#4239);
#1104=VERTEX_POINT('',#4276);
#1105=VERTEX_POINT('',#4277);
#1106=VERTEX_POINT('',#4314);
#1107=VERTEX_POINT('',#4315);
#1108=VERTEX_POINT('',#4352);
#1109=VERTEX_POINT('',#4353);
#1110=VERTEX_POINT('',#4390);
#1111=VERTEX_POINT('',#4391);
#1112=VERTEX_POINT('',#4428);
#1113=VERTEX_POINT('',#4429);
#1114=VERTEX_POINT('',#4466);
#1115=VERTEX_POINT('',#4467);
#1116=VERTEX_POINT('',#4504);
#1117=VERTEX_POINT('',#4505);
#1118=VERTEX_POINT('',#4542);
#1119=VERTEX_POINT('',#4543);
#1120=VERTEX_POINT('',#4580);
#1121=VERTEX_POINT('',#4581);
#1122=VERTEX_POINT('',#4618);
#1123=VERTEX_POINT('',#4619);
#1124=VERTEX_POINT('',#4656);
#1125=VERTEX_POINT('',#4657);
#1126=VERTEX_POINT('',#4694);
#1127=VERTEX_POINT('',#4695);
#1128=VERTEX_POINT('',#4732);
#1129=VERTEX_POINT('',#4733);
#1130=VERTEX_POINT('',#4770);
#1131=VERTEX_POINT('',#4771);
#1132=VERTEX_POINT('',#4808);
#1133=VERTEX_POINT('',#4809);
#1134=VERTEX_POINT('',#4846);
#1135=VERTEX_POINT('',#4847);
#1136=VERTEX_POINT('',#4884);
#1137=VERTEX_POINT('',#4885);
#1138=VERTEX_POINT('',#4922);
#1139=VERTEX_POINT('',#4923);
#1140=VERTEX_POINT('',#4960);
#1141=VERTEX_POINT('',#4961);
#1142=VERTEX_POINT('',#4998);
#1143=VERTEX_POINT('',#4999);
#1144=VERTEX_POINT('',#5036);
#1145=VERTEX_POINT('',#5037);
#1146=VERTEX_POINT('',#5074);
#1147=VERTEX_POINT('',#5075);
#1148=VERTEX_POINT('',#5112);
#1149=VERTEX_POINT('',#5113);
#1150=VERTEX_POINT('',#5150);
#1151=VERTEX_POINT('',#5151);
#1152=VERTEX_POINT('',#5188);
#1153=VERTEX_POINT('',#5189);
#1154=VERTEX_POINT('',#5226);
#1155=VERTEX_POINT('',#5227);
#1156=VERTEX_POINT('',#5264);
#1157=VERTEX_POINT('',#5265);
#1158=VERTEX_POINT('',#5302);
#1159=VERTEX_POINT('',#5303);
#1160=VERTEX_POINT('',#5340);
#1161=VERTEX_POINT('',#5341);
#1162=VERTEX_POINT('',#5378);
#1163=VERTEX_POINT('',#5379);
#1164=VERTEX_POINT('',#5416);
#1165=VERTEX_POINT('',#5417);
#1166=VERTEX_POINT('',#5454);
#1167=VERTEX_POINT('',#5455);
#1168=VERTEX_POINT('',#5492);
#1169=VERTEX_POINT('',#5493);
#1170=VERTEX_POINT('',#5530);
#1171=VERTEX_POINT('',#5531);
#1172=VERTEX_POINT('',#5568);
#1173=VERTEX_POINT('',#5569);
#1174=VERTEX_POINT('',#5606);
#1175=VERTEX_POINT('',#5607);
#1176=VERTEX_POINT('',#5644);
#1177=VERTEX_POINT('',#5645);
#1178=VERTEX_POINT('',#5682);
#1179=VERTEX_POINT('',#5683);
#1180=VERTEX_POINT('',#5720);
#1181=VERTEX_POINT('',#5721);
#1182=VERTEX_POINT('',#5758);
#1183=VERTEX_POINT('',#5759);
#1184=VERTEX_POINT('',#5761);
#1185=VERTEX_POINT('',#5771);
#1186=VERTEX_POINT('',#5783);
#1187=VERTEX_POINT('',#5784);
#1188=VERTEX_POINT('',#5786);
#1189=VERTEX_POINT('',#5792);
#1190=VERTEX_POINT('',#5802);
#1191=VERTEX_POINT('',#5803);
#1192=VERTEX_POINT('',#5840);
#1193=VERTEX_POINT('',#5841);
#1194=VERTEX_POINT('',#5878);
#1195=VERTEX_POINT('',#5879);
#1196=VERTEX_POINT('',#5916);
#1197=VERTEX_POINT('',#5917);
#1198=VERTEX_POINT('',#5954);
#1199=VERTEX_POINT('',#5955);
#1200=VERTEX_POINT('',#5992);
#1201=VERTEX_POINT('',#5993);
#1202=VERTEX_POINT('',#6030);
#1203=VERTEX_POINT('',#6031);
#1204=VERTEX_POINT('',#6068);
#1205=VERTEX_POINT('',#6069);
#1206=VERTEX_POINT('',#6106);
#1207=VERTEX_POINT('',#6107);
#1208=VERTEX_POINT('',#6144);
#1209=VERTEX_POINT('',#6145);
#1210=VERTEX_POINT('',#6182);
#1211=VERTEX_POINT('',#6183);
#1212=VERTEX_POINT('',#6220);
#1213=VERTEX_POINT('',#6221);
#1214=VERTEX_POINT('',#6258);
#1215=VERTEX_POINT('',#6259);
#1216=VERTEX_POINT('',#6296);
#1217=VERTEX_POINT('',#6297);
#1218=VERTEX_POINT('',#6334);
#1219=VERTEX_POINT('',#6335);
#1220=VERTEX_POINT('',#6372);
#1221=VERTEX_POINT('',#6373);
#1222=VERTEX_POINT('',#6410);
#1223=VERTEX_POINT('',#6411);
#1224=VERTEX_POINT('',#6448);
#1225=VERTEX_POINT('',#6449);
#1226=VERTEX_POINT('',#6486);
#1227=VERTEX_POINT('',#6487);
#1228=VERTEX_POINT('',#6524);
#1229=VERTEX_POINT('',#6525);
#1230=VERTEX_POINT('',#6562);
#1231=VERTEX_POINT('',#6563);
#1232=VERTEX_POINT('',#6600);
#1233=VERTEX_POINT('',#6601);
#1234=VERTEX_POINT('',#6638);
#1235=VERTEX_POINT('',#6639);
#1236=VERTEX_POINT('',#6676);
#1237=VERTEX_POINT('',#6677);
#1238=VERTEX_POINT('',#6714);
#1239=VERTEX_POINT('',#6715);
#1240=VERTEX_POINT('',#6752);
#1241=VERTEX_POINT('',#6753);
#1242=VERTEX_POINT('',#6790);
#1243=VERTEX_POINT('',#6791);
#1244=VERTEX_POINT('',#6828);
#1245=VERTEX_POINT('',#6829);
#1246=VERTEX_POINT('',#6866);
#1247=VERTEX_POINT('',#6867);
#1248=VERTEX_POINT('',#6904);
#1249=VERTEX_POINT('',#6905);
#1250=VERTEX_POINT('',#6942);
#1251=VERTEX_POINT('',#6943);
#1252=VERTEX_POINT('',#6980);
#1253=VERTEX_POINT('',#6981);
#1254=VERTEX_POINT('',#7018);
#1255=VERTEX_POINT('',#7019);
#1256=VERTEX_POINT('',#7056);
#1257=VERTEX_POINT('',#7057);
#1258=VERTEX_POINT('',#7094);
#1259=VERTEX_POINT('',#7095);
#1260=VERTEX_POINT('',#7132);
#1261=VERTEX_POINT('',#7133);
#1262=VERTEX_POINT('',#7170);
#1263=VERTEX_POINT('',#7171);
#1264=VERTEX_POINT('',#7208);
#1265=VERTEX_POINT('',#7209);
#1266=VERTEX_POINT('',#7246);
#1267=VERTEX_POINT('',#7247);
#1268=VERTEX_POINT('',#7284);
#1269=VERTEX_POINT('',#7285);
#1270=VERTEX_POINT('',#7322);
#1271=VERTEX_POINT('',#7323);
#1272=VERTEX_POINT('',#7360);
#1273=VERTEX_POINT('',#7361);
#1274=VERTEX_POINT('',#7398);
#1275=VERTEX_POINT('',#7399);
#1276=VERTEX_POINT('',#7436);
#1277=VERTEX_POINT('',#7437);
#1278=VERTEX_POINT('',#7474);
#1279=VERTEX_POINT('',#7475);
#1280=VERTEX_POINT('',#7512);
#1281=VERTEX_POINT('',#7513);
#1282=VERTEX_POINT('',#7550);
#1283=VERTEX_POINT('',#7551);
#1284=VERTEX_POINT('',#7588);
#1285=VERTEX_POINT('',#7590);
#1286=VERTEX_POINT('',#7592);
#1287=VERTEX_POINT('',#7610);
#1288=VERTEX_POINT('',#7612);
#1289=VERTEX_POINT('',#7626);
#1290=VERTEX_POINT('',#7642);
#1291=VERTEX_POINT('',#7643);
#1292=VERTEX_POINT('',#7646);
#1293=VERTEX_POINT('',#7649);
#1294=VERTEX_POINT('',#7650);
#1295=VERTEX_POINT('',#7687);
#1296=VERTEX_POINT('',#7688);
#1297=VERTEX_POINT('',#7761);
#1298=VERTEX_POINT('',#7763);
#1299=VERTEX_POINT('',#7766);
#1300=VERTEX_POINT('',#7770);
#1301=VERTEX_POINT('',#7779);
#1302=VERTEX_POINT('',#11038);
#1303=VERTEX_POINT('',#11043);
#1304=VERTEX_POINT('',#11053);
#1305=VERTEX_POINT('',#11056);
#1306=VERTEX_POINT('',#11058);
#1307=VERTEX_POINT('',#11062);
#1308=VERTEX_POINT('',#11065);
#1309=VERTEX_POINT('',#11076);
#1310=VERTEX_POINT('',#11077);
#1311=VERTEX_POINT('',#11138);
#1312=VERTEX_POINT('',#11142);
#1313=VERTEX_POINT('',#11144);
#1314=VERTEX_POINT('',#11147);
#1315=VERTEX_POINT('',#11149);
#1316=VERTEX_POINT('',#11153);
#1317=VERTEX_POINT('',#11154);
#1318=VERTEX_POINT('',#11218);
#1319=VERTEX_POINT('',#11222);
#1320=VERTEX_POINT('',#11225);
#1321=VERTEX_POINT('',#11229);
#1322=VERTEX_POINT('',#11232);
#1323=VERTEX_POINT('',#11238);
#1324=VERTEX_POINT('',#11240);
#1325=VERTEX_POINT('',#11243);
#1326=VERTEX_POINT('',#11247);
#1327=VERTEX_POINT('',#11251);
#1328=VERTEX_POINT('',#11255);
#1329=VERTEX_POINT('',#11257);
#1330=VERTEX_POINT('',#11262);
#1331=VERTEX_POINT('',#11264);
#1332=VERTEX_POINT('',#11271);
#1333=VERTEX_POINT('',#11273);
#1334=VERTEX_POINT('',#11276);
#1335=VERTEX_POINT('',#11277);
#1336=VERTEX_POINT('',#11282);
#1337=VERTEX_POINT('',#11286);
#1338=VERTEX_POINT('',#11288);
#1339=VERTEX_POINT('',#11292);
#1340=VERTEX_POINT('',#11296);
#1341=VERTEX_POINT('',#11299);
#1342=VERTEX_POINT('',#11301);
#1343=VERTEX_POINT('',#11305);
#1344=VERTEX_POINT('',#11307);
#1345=VERTEX_POINT('',#11312);
#1346=VERTEX_POINT('',#11319);
#1347=VERTEX_POINT('',#11320);
#1348=VERTEX_POINT('',#11322);
#1349=VERTEX_POINT('',#11366);
#1350=VERTEX_POINT('',#11369);
#1351=VERTEX_POINT('',#11373);
#1352=VERTEX_POINT('',#11380);
#1353=VERTEX_POINT('',#11382);
#1354=VERTEX_POINT('',#11384);
#1355=VERTEX_POINT('',#11743);
#1356=VERTEX_POINT('',#11745);
#1357=VERTEX_POINT('',#11787);
#1358=VERTEX_POINT('',#12557);
#1359=VERTEX_POINT('',#12564);
#1360=VERTEX_POINT('',#12568);
#1361=VERTEX_POINT('',#12575);
#1362=VERTEX_POINT('',#13547);
#1363=VERTEX_POINT('',#13548);
#1364=VERTEX_POINT('',#13550);
#1365=VERTEX_POINT('',#13552);
#1366=VERTEX_POINT('',#13556);
#1367=VERTEX_POINT('',#13558);
#1368=VERTEX_POINT('',#13562);
#1369=VERTEX_POINT('',#13564);
#1370=EDGE_CURVE('',#1082,#1083,#780,.T.);
#1371=EDGE_CURVE('',#1083,#1084,#570,.T.);
#1372=EDGE_CURVE('',#1085,#1084,#781,.T.);
#1373=EDGE_CURVE('',#1082,#1085,#571,.T.);
#1374=EDGE_CURVE('',#1086,#1087,#782,.T.);
#1375=EDGE_CURVE('',#1087,#1083,#572,.T.);
#1376=EDGE_CURVE('',#1086,#1082,#573,.T.);
#1377=EDGE_CURVE('',#1088,#1089,#783,.T.);
#1378=EDGE_CURVE('',#1089,#1087,#574,.T.);
#1379=EDGE_CURVE('',#1088,#1086,#575,.T.);
#1380=EDGE_CURVE('',#1090,#1091,#784,.T.);
#1381=EDGE_CURVE('',#1091,#1089,#576,.T.);
#1382=EDGE_CURVE('',#1090,#1088,#577,.T.);
#1383=EDGE_CURVE('',#1092,#1093,#785,.T.);
#1384=EDGE_CURVE('',#1093,#1091,#578,.T.);
#1385=EDGE_CURVE('',#1092,#1090,#579,.T.);
#1386=EDGE_CURVE('',#1094,#1095,#786,.T.);
#1387=EDGE_CURVE('',#1095,#1093,#580,.T.);
#1388=EDGE_CURVE('',#1094,#1092,#581,.T.);
#1389=EDGE_CURVE('',#1096,#1097,#787,.T.);
#1390=EDGE_CURVE('',#1097,#1095,#582,.T.);
#1391=EDGE_CURVE('',#1096,#1094,#583,.T.);
#1392=EDGE_CURVE('',#1098,#1099,#788,.T.);
#1393=EDGE_CURVE('',#1099,#1097,#584,.T.);
#1394=EDGE_CURVE('',#1098,#1096,#585,.T.);
#1395=EDGE_CURVE('',#1100,#1101,#789,.T.);
#1396=EDGE_CURVE('',#1101,#1099,#586,.T.);
#1397=EDGE_CURVE('',#1100,#1098,#587,.T.);
#1398=EDGE_CURVE('',#1102,#1103,#790,.T.);
#1399=EDGE_CURVE('',#1103,#1101,#588,.T.);
#1400=EDGE_CURVE('',#1102,#1100,#589,.T.);
#1401=EDGE_CURVE('',#1104,#1105,#791,.T.);
#1402=EDGE_CURVE('',#1105,#1103,#590,.T.);
#1403=EDGE_CURVE('',#1104,#1102,#591,.T.);
#1404=EDGE_CURVE('',#1106,#1107,#792,.T.);
#1405=EDGE_CURVE('',#1107,#1105,#592,.T.);
#1406=EDGE_CURVE('',#1106,#1104,#593,.T.);
#1407=EDGE_CURVE('',#1108,#1109,#793,.T.);
#1408=EDGE_CURVE('',#1109,#1107,#594,.T.);
#1409=EDGE_CURVE('',#1108,#1106,#595,.T.);
#1410=EDGE_CURVE('',#1110,#1111,#794,.T.);
#1411=EDGE_CURVE('',#1111,#1109,#596,.T.);
#1412=EDGE_CURVE('',#1110,#1108,#597,.T.);
#1413=EDGE_CURVE('',#1112,#1113,#795,.T.);
#1414=EDGE_CURVE('',#1113,#1111,#598,.T.);
#1415=EDGE_CURVE('',#1112,#1110,#599,.T.);
#1416=EDGE_CURVE('',#1114,#1115,#796,.T.);
#1417=EDGE_CURVE('',#1115,#1113,#600,.T.);
#1418=EDGE_CURVE('',#1114,#1112,#601,.T.);
#1419=EDGE_CURVE('',#1116,#1117,#797,.T.);
#1420=EDGE_CURVE('',#1117,#1115,#602,.T.);
#1421=EDGE_CURVE('',#1116,#1114,#603,.T.);
#1422=EDGE_CURVE('',#1118,#1119,#798,.T.);
#1423=EDGE_CURVE('',#1119,#1117,#604,.T.);
#1424=EDGE_CURVE('',#1118,#1116,#605,.T.);
#1425=EDGE_CURVE('',#1120,#1121,#799,.T.);
#1426=EDGE_CURVE('',#1121,#1119,#606,.T.);
#1427=EDGE_CURVE('',#1120,#1118,#607,.T.);
#1428=EDGE_CURVE('',#1122,#1123,#800,.T.);
#1429=EDGE_CURVE('',#1123,#1121,#608,.T.);
#1430=EDGE_CURVE('',#1122,#1120,#609,.T.);
#1431=EDGE_CURVE('',#1124,#1125,#801,.T.);
#1432=EDGE_CURVE('',#1125,#1123,#610,.T.);
#1433=EDGE_CURVE('',#1124,#1122,#611,.T.);
#1434=EDGE_CURVE('',#1126,#1127,#802,.T.);
#1435=EDGE_CURVE('',#1127,#1125,#612,.T.);
#1436=EDGE_CURVE('',#1126,#1124,#613,.T.);
#1437=EDGE_CURVE('',#1128,#1129,#803,.T.);
#1438=EDGE_CURVE('',#1129,#1127,#614,.T.);
#1439=EDGE_CURVE('',#1128,#1126,#615,.T.);
#1440=EDGE_CURVE('',#1130,#1131,#804,.T.);
#1441=EDGE_CURVE('',#1131,#1129,#616,.T.);
#1442=EDGE_CURVE('',#1130,#1128,#617,.T.);
#1443=EDGE_CURVE('',#1132,#1133,#805,.T.);
#1444=EDGE_CURVE('',#1133,#1131,#618,.T.);
#1445=EDGE_CURVE('',#1132,#1130,#619,.T.);
#1446=EDGE_CURVE('',#1134,#1135,#806,.T.);
#1447=EDGE_CURVE('',#1135,#1133,#620,.T.);
#1448=EDGE_CURVE('',#1134,#1132,#621,.T.);
#1449=EDGE_CURVE('',#1136,#1137,#807,.T.);
#1450=EDGE_CURVE('',#1137,#1135,#622,.T.);
#1451=EDGE_CURVE('',#1136,#1134,#623,.T.);
#1452=EDGE_CURVE('',#1138,#1139,#808,.T.);
#1453=EDGE_CURVE('',#1139,#1137,#624,.T.);
#1454=EDGE_CURVE('',#1138,#1136,#625,.T.);
#1455=EDGE_CURVE('',#1140,#1141,#809,.T.);
#1456=EDGE_CURVE('',#1141,#1139,#626,.T.);
#1457=EDGE_CURVE('',#1140,#1138,#627,.T.);
#1458=EDGE_CURVE('',#1142,#1143,#810,.T.);
#1459=EDGE_CURVE('',#1143,#1141,#628,.T.);
#1460=EDGE_CURVE('',#1142,#1140,#629,.T.);
#1461=EDGE_CURVE('',#1144,#1145,#811,.T.);
#1462=EDGE_CURVE('',#1145,#1143,#630,.T.);
#1463=EDGE_CURVE('',#1144,#1142,#631,.T.);
#1464=EDGE_CURVE('',#1146,#1147,#812,.T.);
#1465=EDGE_CURVE('',#1147,#1145,#632,.T.);
#1466=EDGE_CURVE('',#1146,#1144,#633,.T.);
#1467=EDGE_CURVE('',#1148,#1149,#813,.T.);
#1468=EDGE_CURVE('',#1149,#1147,#634,.T.);
#1469=EDGE_CURVE('',#1148,#1146,#635,.T.);
#1470=EDGE_CURVE('',#1150,#1151,#814,.T.);
#1471=EDGE_CURVE('',#1151,#1149,#636,.T.);
#1472=EDGE_CURVE('',#1150,#1148,#637,.T.);
#1473=EDGE_CURVE('',#1152,#1153,#815,.T.);
#1474=EDGE_CURVE('',#1153,#1151,#638,.T.);
#1475=EDGE_CURVE('',#1152,#1150,#639,.T.);
#1476=EDGE_CURVE('',#1154,#1155,#816,.T.);
#1477=EDGE_CURVE('',#1155,#1153,#640,.T.);
#1478=EDGE_CURVE('',#1154,#1152,#641,.T.);
#1479=EDGE_CURVE('',#1156,#1157,#817,.T.);
#1480=EDGE_CURVE('',#1157,#1155,#642,.T.);
#1481=EDGE_CURVE('',#1156,#1154,#643,.T.);
#1482=EDGE_CURVE('',#1158,#1159,#818,.T.);
#1483=EDGE_CURVE('',#1159,#1157,#644,.T.);
#1484=EDGE_CURVE('',#1158,#1156,#645,.T.);
#1485=EDGE_CURVE('',#1160,#1161,#819,.T.);
#1486=EDGE_CURVE('',#1161,#1159,#646,.T.);
#1487=EDGE_CURVE('',#1160,#1158,#647,.T.);
#1488=EDGE_CURVE('',#1162,#1163,#820,.T.);
#1489=EDGE_CURVE('',#1163,#1161,#648,.T.);
#1490=EDGE_CURVE('',#1162,#1160,#649,.T.);
#1491=EDGE_CURVE('',#1164,#1165,#821,.T.);
#1492=EDGE_CURVE('',#1165,#1163,#650,.T.);
#1493=EDGE_CURVE('',#1164,#1162,#651,.T.);
#1494=EDGE_CURVE('',#1166,#1167,#822,.T.);
#1495=EDGE_CURVE('',#1167,#1165,#652,.T.);
#1496=EDGE_CURVE('',#1166,#1164,#653,.T.);
#1497=EDGE_CURVE('',#1168,#1169,#823,.T.);
#1498=EDGE_CURVE('',#1169,#1167,#654,.T.);
#1499=EDGE_CURVE('',#1168,#1166,#655,.T.);
#1500=EDGE_CURVE('',#1170,#1171,#824,.T.);
#1501=EDGE_CURVE('',#1171,#1169,#656,.T.);
#1502=EDGE_CURVE('',#1170,#1168,#657,.T.);
#1503=EDGE_CURVE('',#1172,#1173,#825,.T.);
#1504=EDGE_CURVE('',#1173,#1171,#658,.T.);
#1505=EDGE_CURVE('',#1172,#1170,#659,.T.);
#1506=EDGE_CURVE('',#1174,#1175,#826,.T.);
#1507=EDGE_CURVE('',#1175,#1173,#660,.T.);
#1508=EDGE_CURVE('',#1174,#1172,#661,.T.);
#1509=EDGE_CURVE('',#1176,#1177,#827,.T.);
#1510=EDGE_CURVE('',#1177,#1175,#662,.T.);
#1511=EDGE_CURVE('',#1176,#1174,#663,.T.);
#1512=EDGE_CURVE('',#1178,#1179,#828,.T.);
#1513=EDGE_CURVE('',#1179,#1177,#664,.T.);
#1514=EDGE_CURVE('',#1178,#1176,#665,.T.);
#1515=EDGE_CURVE('',#1180,#1181,#829,.T.);
#1516=EDGE_CURVE('',#1181,#1179,#666,.T.);
#1517=EDGE_CURVE('',#1180,#1178,#667,.T.);
#1518=EDGE_CURVE('',#1182,#1183,#830,.T.);
#1519=EDGE_CURVE('',#1184,#1182,#668,.T.);
#1520=EDGE_CURVE('',#1185,#1184,#831,.T.);
#1521=EDGE_CURVE('',#1185,#1183,#669,.T.);
#1522=EDGE_CURVE('',#1186,#1187,#832,.T.);
#1523=EDGE_CURVE('',#1187,#1188,#670,.T.);
#1524=EDGE_CURVE('',#1189,#1188,#149,.T.);
#1525=EDGE_CURVE('',#1186,#1189,#671,.T.);
#1526=EDGE_CURVE('',#1190,#1191,#833,.T.);
#1527=EDGE_CURVE('',#1191,#1187,#672,.T.);
#1528=EDGE_CURVE('',#1190,#1186,#673,.T.);
#1529=EDGE_CURVE('',#1192,#1193,#834,.T.);
#1530=EDGE_CURVE('',#1193,#1191,#674,.T.);
#1531=EDGE_CURVE('',#1192,#1190,#675,.T.);
#1532=EDGE_CURVE('',#1194,#1195,#835,.T.);
#1533=EDGE_CURVE('',#1195,#1193,#676,.T.);
#1534=EDGE_CURVE('',#1194,#1192,#677,.T.);
#1535=EDGE_CURVE('',#1196,#1197,#836,.T.);
#1536=EDGE_CURVE('',#1197,#1195,#678,.T.);
#1537=EDGE_CURVE('',#1196,#1194,#679,.T.);
#1538=EDGE_CURVE('',#1198,#1199,#837,.T.);
#1539=EDGE_CURVE('',#1199,#1197,#680,.T.);
#1540=EDGE_CURVE('',#1198,#1196,#681,.T.);
#1541=EDGE_CURVE('',#1200,#1201,#838,.T.);
#1542=EDGE_CURVE('',#1201,#1199,#682,.T.);
#1543=EDGE_CURVE('',#1200,#1198,#683,.T.);
#1544=EDGE_CURVE('',#1202,#1203,#839,.T.);
#1545=EDGE_CURVE('',#1203,#1201,#684,.T.);
#1546=EDGE_CURVE('',#1202,#1200,#685,.T.);
#1547=EDGE_CURVE('',#1204,#1205,#840,.T.);
#1548=EDGE_CURVE('',#1205,#1203,#686,.T.);
#1549=EDGE_CURVE('',#1204,#1202,#687,.T.);
#1550=EDGE_CURVE('',#1206,#1207,#841,.T.);
#1551=EDGE_CURVE('',#1207,#1205,#688,.T.);
#1552=EDGE_CURVE('',#1206,#1204,#689,.T.);
#1553=EDGE_CURVE('',#1208,#1209,#842,.T.);
#1554=EDGE_CURVE('',#1209,#1207,#690,.T.);
#1555=EDGE_CURVE('',#1208,#1206,#691,.T.);
#1556=EDGE_CURVE('',#1210,#1211,#843,.T.);
#1557=EDGE_CURVE('',#1211,#1209,#692,.T.);
#1558=EDGE_CURVE('',#1210,#1208,#693,.T.);
#1559=EDGE_CURVE('',#1212,#1213,#844,.T.);
#1560=EDGE_CURVE('',#1213,#1211,#694,.T.);
#1561=EDGE_CURVE('',#1212,#1210,#695,.T.);
#1562=EDGE_CURVE('',#1214,#1215,#845,.T.);
#1563=EDGE_CURVE('',#1215,#1213,#696,.T.);
#1564=EDGE_CURVE('',#1214,#1212,#697,.T.);
#1565=EDGE_CURVE('',#1216,#1217,#846,.T.);
#1566=EDGE_CURVE('',#1217,#1215,#698,.T.);
#1567=EDGE_CURVE('',#1216,#1214,#699,.T.);
#1568=EDGE_CURVE('',#1218,#1219,#847,.T.);
#1569=EDGE_CURVE('',#1219,#1217,#700,.T.);
#1570=EDGE_CURVE('',#1218,#1216,#701,.T.);
#1571=EDGE_CURVE('',#1220,#1221,#848,.T.);
#1572=EDGE_CURVE('',#1221,#1219,#702,.T.);
#1573=EDGE_CURVE('',#1220,#1218,#703,.T.);
#1574=EDGE_CURVE('',#1222,#1223,#849,.T.);
#1575=EDGE_CURVE('',#1223,#1221,#704,.T.);
#1576=EDGE_CURVE('',#1222,#1220,#705,.T.);
#1577=EDGE_CURVE('',#1224,#1225,#850,.T.);
#1578=EDGE_CURVE('',#1225,#1223,#706,.T.);
#1579=EDGE_CURVE('',#1224,#1222,#707,.T.);
#1580=EDGE_CURVE('',#1226,#1227,#851,.T.);
#1581=EDGE_CURVE('',#1227,#1225,#708,.T.);
#1582=EDGE_CURVE('',#1226,#1224,#709,.T.);
#1583=EDGE_CURVE('',#1228,#1229,#852,.T.);
#1584=EDGE_CURVE('',#1229,#1227,#710,.T.);
#1585=EDGE_CURVE('',#1228,#1226,#711,.T.);
#1586=EDGE_CURVE('',#1230,#1231,#853,.T.);
#1587=EDGE_CURVE('',#1231,#1229,#712,.T.);
#1588=EDGE_CURVE('',#1230,#1228,#713,.T.);
#1589=EDGE_CURVE('',#1232,#1233,#854,.T.);
#1590=EDGE_CURVE('',#1233,#1231,#714,.T.);
#1591=EDGE_CURVE('',#1232,#1230,#715,.T.);
#1592=EDGE_CURVE('',#1234,#1235,#855,.T.);
#1593=EDGE_CURVE('',#1235,#1233,#716,.T.);
#1594=EDGE_CURVE('',#1234,#1232,#717,.T.);
#1595=EDGE_CURVE('',#1236,#1237,#856,.T.);
#1596=EDGE_CURVE('',#1237,#1235,#718,.T.);
#1597=EDGE_CURVE('',#1236,#1234,#719,.T.);
#1598=EDGE_CURVE('',#1238,#1239,#857,.T.);
#1599=EDGE_CURVE('',#1239,#1237,#720,.T.);
#1600=EDGE_CURVE('',#1238,#1236,#721,.T.);
#1601=EDGE_CURVE('',#1240,#1241,#858,.T.);
#1602=EDGE_CURVE('',#1241,#1239,#722,.T.);
#1603=EDGE_CURVE('',#1240,#1238,#723,.T.);
#1604=EDGE_CURVE('',#1242,#1243,#859,.T.);
#1605=EDGE_CURVE('',#1243,#1241,#724,.T.);
#1606=EDGE_CURVE('',#1242,#1240,#725,.T.);
#1607=EDGE_CURVE('',#1244,#1245,#860,.T.);
#1608=EDGE_CURVE('',#1245,#1243,#726,.T.);
#1609=EDGE_CURVE('',#1244,#1242,#727,.T.);
#1610=EDGE_CURVE('',#1246,#1247,#861,.T.);
#1611=EDGE_CURVE('',#1247,#1245,#728,.T.);
#1612=EDGE_CURVE('',#1246,#1244,#729,.T.);
#1613=EDGE_CURVE('',#1248,#1249,#862,.T.);
#1614=EDGE_CURVE('',#1249,#1247,#730,.T.);
#1615=EDGE_CURVE('',#1248,#1246,#731,.T.);
#1616=EDGE_CURVE('',#1250,#1251,#863,.T.);
#1617=EDGE_CURVE('',#1251,#1249,#732,.T.);
#1618=EDGE_CURVE('',#1250,#1248,#733,.T.);
#1619=EDGE_CURVE('',#1252,#1253,#864,.T.);
#1620=EDGE_CURVE('',#1253,#1251,#734,.T.);
#1621=EDGE_CURVE('',#1252,#1250,#735,.T.);
#1622=EDGE_CURVE('',#1254,#1255,#865,.T.);
#1623=EDGE_CURVE('',#1255,#1253,#736,.T.);
#1624=EDGE_CURVE('',#1254,#1252,#737,.T.);
#1625=EDGE_CURVE('',#1256,#1257,#866,.T.);
#1626=EDGE_CURVE('',#1257,#1255,#738,.T.);
#1627=EDGE_CURVE('',#1256,#1254,#739,.T.);
#1628=EDGE_CURVE('',#1258,#1259,#867,.T.);
#1629=EDGE_CURVE('',#1259,#1257,#740,.T.);
#1630=EDGE_CURVE('',#1258,#1256,#741,.T.);
#1631=EDGE_CURVE('',#1260,#1261,#868,.T.);
#1632=EDGE_CURVE('',#1261,#1259,#742,.T.);
#1633=EDGE_CURVE('',#1260,#1258,#743,.T.);
#1634=EDGE_CURVE('',#1262,#1263,#869,.T.);
#1635=EDGE_CURVE('',#1263,#1261,#744,.T.);
#1636=EDGE_CURVE('',#1262,#1260,#745,.T.);
#1637=EDGE_CURVE('',#1264,#1265,#870,.T.);
#1638=EDGE_CURVE('',#1265,#1263,#746,.T.);
#1639=EDGE_CURVE('',#1264,#1262,#747,.T.);
#1640=EDGE_CURVE('',#1266,#1267,#871,.T.);
#1641=EDGE_CURVE('',#1267,#1265,#748,.T.);
#1642=EDGE_CURVE('',#1266,#1264,#749,.T.);
#1643=EDGE_CURVE('',#1268,#1269,#872,.T.);
#1644=EDGE_CURVE('',#1269,#1267,#750,.T.);
#1645=EDGE_CURVE('',#1268,#1266,#751,.T.);
#1646=EDGE_CURVE('',#1270,#1271,#873,.T.);
#1647=EDGE_CURVE('',#1271,#1269,#752,.T.);
#1648=EDGE_CURVE('',#1270,#1268,#753,.T.);
#1649=EDGE_CURVE('',#1272,#1273,#874,.T.);
#1650=EDGE_CURVE('',#1273,#1271,#754,.T.);
#1651=EDGE_CURVE('',#1272,#1270,#755,.T.);
#1652=EDGE_CURVE('',#1274,#1275,#875,.T.);
#1653=EDGE_CURVE('',#1275,#1273,#756,.T.);
#1654=EDGE_CURVE('',#1274,#1272,#757,.T.);
#1655=EDGE_CURVE('',#1276,#1277,#876,.T.);
#1656=EDGE_CURVE('',#1277,#1275,#758,.T.);
#1657=EDGE_CURVE('',#1276,#1274,#759,.T.);
#1658=EDGE_CURVE('',#1278,#1279,#877,.T.);
#1659=EDGE_CURVE('',#1279,#1277,#760,.T.);
#1660=EDGE_CURVE('',#1278,#1276,#761,.T.);
#1661=EDGE_CURVE('',#1280,#1281,#878,.T.);
#1662=EDGE_CURVE('',#1281,#1279,#762,.T.);
#1663=EDGE_CURVE('',#1280,#1278,#763,.T.);
#1664=EDGE_CURVE('',#1282,#1283,#879,.T.);
#1665=EDGE_CURVE('',#1283,#1281,#764,.T.);
#1666=EDGE_CURVE('',#1282,#1280,#765,.T.);
#1667=EDGE_CURVE('',#1284,#1284,#150,.T.);
#1668=EDGE_CURVE('',#1284,#1285,#880,.T.);
#1669=EDGE_CURVE('',#1285,#1286,#766,.T.);
#1670=EDGE_CURVE('',#1287,#1286,#881,.T.);
#1671=EDGE_CURVE('',#1288,#1287,#767,.T.);
#1672=EDGE_CURVE('',#1289,#1288,#882,.T.);
#1673=EDGE_CURVE('',#1289,#1285,#768,.T.);
#1674=EDGE_CURVE('',#1290,#1291,#151,.T.);
#1675=EDGE_CURVE('',#1291,#1290,#152,.T.);
#1676=EDGE_CURVE('',#1290,#1292,#883,.T.);
#1677=EDGE_CURVE('',#1292,#1292,#153,.F.);
#1678=EDGE_CURVE('',#1293,#1294,#135,.T.);
#1679=EDGE_CURVE('',#1294,#1293,#136,.T.);
#1680=EDGE_CURVE('',#1295,#1296,#137,.T.);
#1681=EDGE_CURVE('',#1296,#1295,#138,.T.);
#1682=EDGE_CURVE('',#1286,#1283,#769,.T.);
#1683=EDGE_CURVE('',#1287,#1282,#770,.T.);
#1684=EDGE_CURVE('',#1297,#1297,#154,.T.);
#1685=EDGE_CURVE('',#1298,#1298,#155,.T.);
#1686=EDGE_CURVE('',#1299,#1299,#156,.F.);
#1687=EDGE_CURVE('',#1188,#1189,#157,.T.);
#1688=EDGE_CURVE('',#1300,#1300,#158,.T.);
#1689=EDGE_CURVE('',#1292,#1297,#884,.T.);
#1690=EDGE_CURVE('',#1184,#1289,#885,.T.);
#1691=EDGE_CURVE('',#1288,#1185,#886,.T.);
#1692=EDGE_CURVE('',#1188,#1085,#887,.T.);
#1693=EDGE_CURVE('',#1084,#1301,#888,.T.);
#1694=EDGE_CURVE('',#1301,#1188,#889,.T.);
#1695=EDGE_CURVE('',#1182,#1180,#771,.T.);
#1696=EDGE_CURVE('',#1183,#1181,#772,.T.);
#1697=EDGE_CURVE('',#1189,#1301,#773,.T.);
#1698=EDGE_CURVE('',#1294,#1302,#890,.T.);
#1699=EDGE_CURVE('',#1302,#1302,#159,.T.);
#1700=EDGE_CURVE('',#1296,#1303,#891,.T.);
#1701=EDGE_CURVE('',#1303,#1303,#160,.T.);
#1702=EDGE_CURVE('',#1300,#1298,#892,.T.);
#1703=EDGE_CURVE('',#1291,#1299,#893,.T.);
#1704=EDGE_CURVE('',#1304,#1304,#161,.F.);
#1705=EDGE_CURVE('',#1305,#1305,#162,.T.);
#1706=EDGE_CURVE('',#1305,#1306,#894,.T.);
#1707=EDGE_CURVE('',#1306,#1306,#163,.T.);
#1708=EDGE_CURVE('',#1307,#1307,#164,.T.);
#1709=EDGE_CURVE('',#1308,#1308,#165,.T.);
#1710=EDGE_CURVE('',#1308,#1307,#895,.T.);
#1711=EDGE_CURVE('',#1306,#1304,#896,.T.);
#1712=EDGE_CURVE('',#1309,#1310,#139,.T.);
#1713=EDGE_CURVE('',#1310,#1309,#140,.T.);
#1714=EDGE_CURVE('',#1310,#1311,#897,.T.);
#1715=EDGE_CURVE('',#1311,#1311,#166,.F.);
#1716=EDGE_CURVE('',#1312,#1312,#167,.T.);
#1717=EDGE_CURVE('',#1313,#1313,#168,.T.);
#1718=EDGE_CURVE('',#1314,#1314,#169,.T.);
#1719=EDGE_CURVE('',#1315,#1315,#170,.T.);
#1720=EDGE_CURVE('',#1314,#1312,#898,.T.);
#1721=EDGE_CURVE('',#1316,#1317,#141,.T.);
#1722=EDGE_CURVE('',#1317,#1316,#142,.T.);
#1723=EDGE_CURVE('',#1313,#1315,#899,.T.);
#1724=EDGE_CURVE('',#1318,#1318,#171,.T.);
#1725=EDGE_CURVE('',#1318,#1317,#900,.T.);
#1726=EDGE_CURVE('',#1319,#1319,#172,.T.);
#1727=EDGE_CURVE('',#1320,#1320,#173,.T.);
#1728=EDGE_CURVE('',#1320,#1319,#901,.T.);
#1729=EDGE_CURVE('',#1321,#1321,#174,.T.);
#1730=EDGE_CURVE('',#1321,#1322,#902,.T.);
#1731=EDGE_CURVE('',#1322,#1322,#175,.T.);
#1732=EDGE_CURVE('',#1323,#1323,#176,.T.);
#1733=EDGE_CURVE('',#1324,#1324,#177,.T.);
#1734=EDGE_CURVE('',#1323,#1325,#903,.T.);
#1735=EDGE_CURVE('',#1325,#1325,#178,.T.);
#1736=EDGE_CURVE('',#1326,#1326,#179,.T.);
#1737=EDGE_CURVE('',#1326,#1324,#904,.T.);
#1738=EDGE_CURVE('',#1327,#1327,#180,.F.);
#1739=EDGE_CURVE('',#1327,#1326,#905,.T.);
#1740=EDGE_CURVE('',#1328,#1328,#181,.T.);
#1741=EDGE_CURVE('',#1328,#1329,#906,.T.);
#1742=EDGE_CURVE('',#1329,#1329,#182,.T.);
#1743=EDGE_CURVE('',#1330,#1330,#183,.T.);
#1744=EDGE_CURVE('',#1330,#1331,#907,.T.);
#1745=EDGE_CURVE('',#1331,#1331,#184,.T.);
#1746=EDGE_CURVE('',#1332,#1332,#185,.T.);
#1747=EDGE_CURVE('',#1333,#1333,#186,.T.);
#1748=EDGE_CURVE('',#1334,#1335,#187,.T.);
#1749=EDGE_CURVE('',#1335,#1334,#188,.T.);
#1750=EDGE_CURVE('',#1334,#1332,#189,.T.);
#1751=EDGE_CURVE('',#1336,#1336,#190,.T.);
#1752=EDGE_CURVE('',#1336,#1335,#908,.T.);
#1753=EDGE_CURVE('',#1333,#1337,#191,.T.);
#1754=EDGE_CURVE('',#1338,#1337,#192,.T.);
#1755=EDGE_CURVE('',#1337,#1338,#193,.T.);
#1756=EDGE_CURVE('',#1338,#1339,#909,.T.);
#1757=EDGE_CURVE('',#1339,#1339,#194,.T.);
#1758=EDGE_CURVE('',#1340,#1340,#195,.T.);
#1759=EDGE_CURVE('',#1341,#1341,#196,.T.);
#1760=EDGE_CURVE('',#1341,#1342,#910,.T.);
#1761=EDGE_CURVE('',#1342,#1342,#197,.T.);
#1762=EDGE_CURVE('',#1343,#1343,#198,.T.);
#1763=EDGE_CURVE('',#1343,#1344,#911,.T.);
#1764=EDGE_CURVE('',#1344,#1344,#199,.T.);
#1765=EDGE_CURVE('',#1345,#1345,#200,.T.);
#1766=EDGE_CURVE('',#1345,#1340,#912,.T.);
#1767=EDGE_CURVE('',#1346,#1347,#913,.T.);
#1768=EDGE_CURVE('',#1348,#1346,#774,.T.);
#1769=EDGE_CURVE('',#1348,#1349,#914,.T.);
#1770=EDGE_CURVE('',#1349,#1349,#201,.T.);
#1771=EDGE_CURVE('',#1350,#1348,#775,.T.);
#1772=EDGE_CURVE('',#1350,#1351,#202,.T.);
#1773=EDGE_CURVE('',#1351,#1347,#143,.T.);
#1774=EDGE_CURVE('',#1352,#1352,#203,.T.);
#1775=EDGE_CURVE('',#1352,#1353,#915,.T.);
#1776=EDGE_CURVE('',#1353,#1354,#144,.T.);
#1777=EDGE_CURVE('',#1354,#1355,#204,.T.);
#1778=EDGE_CURVE('',#1356,#1355,#776,.T.);
#1779=EDGE_CURVE('',#1356,#1357,#916,.T.);
#1780=EDGE_CURVE('',#1357,#1353,#145,.T.);
#1781=EDGE_CURVE('',#1346,#1356,#777,.T.);
#1782=EDGE_CURVE('',#1347,#1357,#146,.T.);
#1783=EDGE_CURVE('',#1351,#1358,#147,.T.);
#1784=EDGE_CURVE('',#1359,#1350,#917,.T.);
#1785=EDGE_CURVE('',#1358,#1359,#918,.T.);
#1786=EDGE_CURVE('',#1360,#1354,#148,.T.);
#1787=EDGE_CURVE('',#1361,#1360,#919,.T.);
#1788=EDGE_CURVE('',#1355,#1361,#920,.T.);
#1789=EDGE_CURVE('',#1358,#1360,#778,.T.);
#1790=EDGE_CURVE('',#1359,#1361,#779,.T.);
#1791=EDGE_CURVE('',#1362,#1363,#205,.T.);
#1792=EDGE_CURVE('',#1364,#1363,#921,.T.);
#1793=EDGE_CURVE('',#1365,#1364,#206,.T.);
#1794=EDGE_CURVE('',#1365,#1362,#922,.T.);
#1795=EDGE_CURVE('',#1363,#1366,#923,.T.);
#1796=EDGE_CURVE('',#1367,#1366,#924,.T.);
#1797=EDGE_CURVE('',#1364,#1367,#925,.T.);
#1798=EDGE_CURVE('',#1366,#1368,#926,.T.);
#1799=EDGE_CURVE('',#1369,#1368,#927,.T.);
#1800=EDGE_CURVE('',#1367,#1369,#928,.T.);
#1801=EDGE_CURVE('',#1368,#1362,#929,.T.);
#1802=EDGE_CURVE('',#1369,#1365,#930,.T.);
#1803=ORIENTED_EDGE('',*,*,#1370,.T.);
#1804=ORIENTED_EDGE('',*,*,#1371,.T.);
#1805=ORIENTED_EDGE('',*,*,#1372,.F.);
#1806=ORIENTED_EDGE('',*,*,#1373,.F.);
#1807=ORIENTED_EDGE('',*,*,#1374,.T.);
#1808=ORIENTED_EDGE('',*,*,#1375,.T.);
#1809=ORIENTED_EDGE('',*,*,#1370,.F.);
#1810=ORIENTED_EDGE('',*,*,#1376,.F.);
#1811=ORIENTED_EDGE('',*,*,#1377,.T.);
#1812=ORIENTED_EDGE('',*,*,#1378,.T.);
#1813=ORIENTED_EDGE('',*,*,#1374,.F.);
#1814=ORIENTED_EDGE('',*,*,#1379,.F.);
#1815=ORIENTED_EDGE('',*,*,#1380,.T.);
#1816=ORIENTED_EDGE('',*,*,#1381,.T.);
#1817=ORIENTED_EDGE('',*,*,#1377,.F.);
#1818=ORIENTED_EDGE('',*,*,#1382,.F.);
#1819=ORIENTED_EDGE('',*,*,#1383,.T.);
#1820=ORIENTED_EDGE('',*,*,#1384,.T.);
#1821=ORIENTED_EDGE('',*,*,#1380,.F.);
#1822=ORIENTED_EDGE('',*,*,#1385,.F.);
#1823=ORIENTED_EDGE('',*,*,#1386,.T.);
#1824=ORIENTED_EDGE('',*,*,#1387,.T.);
#1825=ORIENTED_EDGE('',*,*,#1383,.F.);
#1826=ORIENTED_EDGE('',*,*,#1388,.F.);
#1827=ORIENTED_EDGE('',*,*,#1389,.T.);
#1828=ORIENTED_EDGE('',*,*,#1390,.T.);
#1829=ORIENTED_EDGE('',*,*,#1386,.F.);
#1830=ORIENTED_EDGE('',*,*,#1391,.F.);
#1831=ORIENTED_EDGE('',*,*,#1392,.T.);
#1832=ORIENTED_EDGE('',*,*,#1393,.T.);
#1833=ORIENTED_EDGE('',*,*,#1389,.F.);
#1834=ORIENTED_EDGE('',*,*,#1394,.F.);
#1835=ORIENTED_EDGE('',*,*,#1395,.T.);
#1836=ORIENTED_EDGE('',*,*,#1396,.T.);
#1837=ORIENTED_EDGE('',*,*,#1392,.F.);
#1838=ORIENTED_EDGE('',*,*,#1397,.F.);
#1839=ORIENTED_EDGE('',*,*,#1398,.T.);
#1840=ORIENTED_EDGE('',*,*,#1399,.T.);
#1841=ORIENTED_EDGE('',*,*,#1395,.F.);
#1842=ORIENTED_EDGE('',*,*,#1400,.F.);
#1843=ORIENTED_EDGE('',*,*,#1401,.T.);
#1844=ORIENTED_EDGE('',*,*,#1402,.T.);
#1845=ORIENTED_EDGE('',*,*,#1398,.F.);
#1846=ORIENTED_EDGE('',*,*,#1403,.F.);
#1847=ORIENTED_EDGE('',*,*,#1404,.T.);
#1848=ORIENTED_EDGE('',*,*,#1405,.T.);
#1849=ORIENTED_EDGE('',*,*,#1401,.F.);
#1850=ORIENTED_EDGE('',*,*,#1406,.F.);
#1851=ORIENTED_EDGE('',*,*,#1407,.T.);
#1852=ORIENTED_EDGE('',*,*,#1408,.T.);
#1853=ORIENTED_EDGE('',*,*,#1404,.F.);
#1854=ORIENTED_EDGE('',*,*,#1409,.F.);
#1855=ORIENTED_EDGE('',*,*,#1410,.T.);
#1856=ORIENTED_EDGE('',*,*,#1411,.T.);
#1857=ORIENTED_EDGE('',*,*,#1407,.F.);
#1858=ORIENTED_EDGE('',*,*,#1412,.F.);
#1859=ORIENTED_EDGE('',*,*,#1413,.T.);
#1860=ORIENTED_EDGE('',*,*,#1414,.T.);
#1861=ORIENTED_EDGE('',*,*,#1410,.F.);
#1862=ORIENTED_EDGE('',*,*,#1415,.F.);
#1863=ORIENTED_EDGE('',*,*,#1416,.T.);
#1864=ORIENTED_EDGE('',*,*,#1417,.T.);
#1865=ORIENTED_EDGE('',*,*,#1413,.F.);
#1866=ORIENTED_EDGE('',*,*,#1418,.F.);
#1867=ORIENTED_EDGE('',*,*,#1419,.T.);
#1868=ORIENTED_EDGE('',*,*,#1420,.T.);
#1869=ORIENTED_EDGE('',*,*,#1416,.F.);
#1870=ORIENTED_EDGE('',*,*,#1421,.F.);
#1871=ORIENTED_EDGE('',*,*,#1422,.T.);
#1872=ORIENTED_EDGE('',*,*,#1423,.T.);
#1873=ORIENTED_EDGE('',*,*,#1419,.F.);
#1874=ORIENTED_EDGE('',*,*,#1424,.F.);
#1875=ORIENTED_EDGE('',*,*,#1425,.T.);
#1876=ORIENTED_EDGE('',*,*,#1426,.T.);
#1877=ORIENTED_EDGE('',*,*,#1422,.F.);
#1878=ORIENTED_EDGE('',*,*,#1427,.F.);
#1879=ORIENTED_EDGE('',*,*,#1428,.T.);
#1880=ORIENTED_EDGE('',*,*,#1429,.T.);
#1881=ORIENTED_EDGE('',*,*,#1425,.F.);
#1882=ORIENTED_EDGE('',*,*,#1430,.F.);
#1883=ORIENTED_EDGE('',*,*,#1431,.T.);
#1884=ORIENTED_EDGE('',*,*,#1432,.T.);
#1885=ORIENTED_EDGE('',*,*,#1428,.F.);
#1886=ORIENTED_EDGE('',*,*,#1433,.F.);
#1887=ORIENTED_EDGE('',*,*,#1434,.T.);
#1888=ORIENTED_EDGE('',*,*,#1435,.T.);
#1889=ORIENTED_EDGE('',*,*,#1431,.F.);
#1890=ORIENTED_EDGE('',*,*,#1436,.F.);
#1891=ORIENTED_EDGE('',*,*,#1437,.T.);
#1892=ORIENTED_EDGE('',*,*,#1438,.T.);
#1893=ORIENTED_EDGE('',*,*,#1434,.F.);
#1894=ORIENTED_EDGE('',*,*,#1439,.F.);
#1895=ORIENTED_EDGE('',*,*,#1440,.T.);
#1896=ORIENTED_EDGE('',*,*,#1441,.T.);
#1897=ORIENTED_EDGE('',*,*,#1437,.F.);
#1898=ORIENTED_EDGE('',*,*,#1442,.F.);
#1899=ORIENTED_EDGE('',*,*,#1443,.T.);
#1900=ORIENTED_EDGE('',*,*,#1444,.T.);
#1901=ORIENTED_EDGE('',*,*,#1440,.F.);
#1902=ORIENTED_EDGE('',*,*,#1445,.F.);
#1903=ORIENTED_EDGE('',*,*,#1446,.T.);
#1904=ORIENTED_EDGE('',*,*,#1447,.T.);
#1905=ORIENTED_EDGE('',*,*,#1443,.F.);
#1906=ORIENTED_EDGE('',*,*,#1448,.F.);
#1907=ORIENTED_EDGE('',*,*,#1449,.T.);
#1908=ORIENTED_EDGE('',*,*,#1450,.T.);
#1909=ORIENTED_EDGE('',*,*,#1446,.F.);
#1910=ORIENTED_EDGE('',*,*,#1451,.F.);
#1911=ORIENTED_EDGE('',*,*,#1452,.T.);
#1912=ORIENTED_EDGE('',*,*,#1453,.T.);
#1913=ORIENTED_EDGE('',*,*,#1449,.F.);
#1914=ORIENTED_EDGE('',*,*,#1454,.F.);
#1915=ORIENTED_EDGE('',*,*,#1455,.T.);
#1916=ORIENTED_EDGE('',*,*,#1456,.T.);
#1917=ORIENTED_EDGE('',*,*,#1452,.F.);
#1918=ORIENTED_EDGE('',*,*,#1457,.F.);
#1919=ORIENTED_EDGE('',*,*,#1458,.T.);
#1920=ORIENTED_EDGE('',*,*,#1459,.T.);
#1921=ORIENTED_EDGE('',*,*,#1455,.F.);
#1922=ORIENTED_EDGE('',*,*,#1460,.F.);
#1923=ORIENTED_EDGE('',*,*,#1461,.T.);
#1924=ORIENTED_EDGE('',*,*,#1462,.T.);
#1925=ORIENTED_EDGE('',*,*,#1458,.F.);
#1926=ORIENTED_EDGE('',*,*,#1463,.F.);
#1927=ORIENTED_EDGE('',*,*,#1464,.T.);
#1928=ORIENTED_EDGE('',*,*,#1465,.T.);
#1929=ORIENTED_EDGE('',*,*,#1461,.F.);
#1930=ORIENTED_EDGE('',*,*,#1466,.F.);
#1931=ORIENTED_EDGE('',*,*,#1467,.T.);
#1932=ORIENTED_EDGE('',*,*,#1468,.T.);
#1933=ORIENTED_EDGE('',*,*,#1464,.F.);
#1934=ORIENTED_EDGE('',*,*,#1469,.F.);
#1935=ORIENTED_EDGE('',*,*,#1470,.T.);
#1936=ORIENTED_EDGE('',*,*,#1471,.T.);
#1937=ORIENTED_EDGE('',*,*,#1467,.F.);
#1938=ORIENTED_EDGE('',*,*,#1472,.F.);
#1939=ORIENTED_EDGE('',*,*,#1473,.T.);
#1940=ORIENTED_EDGE('',*,*,#1474,.T.);
#1941=ORIENTED_EDGE('',*,*,#1470,.F.);
#1942=ORIENTED_EDGE('',*,*,#1475,.F.);
#1943=ORIENTED_EDGE('',*,*,#1476,.T.);
#1944=ORIENTED_EDGE('',*,*,#1477,.T.);
#1945=ORIENTED_EDGE('',*,*,#1473,.F.);
#1946=ORIENTED_EDGE('',*,*,#1478,.F.);
#1947=ORIENTED_EDGE('',*,*,#1479,.T.);
#1948=ORIENTED_EDGE('',*,*,#1480,.T.);
#1949=ORIENTED_EDGE('',*,*,#1476,.F.);
#1950=ORIENTED_EDGE('',*,*,#1481,.F.);
#1951=ORIENTED_EDGE('',*,*,#1482,.T.);
#1952=ORIENTED_EDGE('',*,*,#1483,.T.);
#1953=ORIENTED_EDGE('',*,*,#1479,.F.);
#1954=ORIENTED_EDGE('',*,*,#1484,.F.);
#1955=ORIENTED_EDGE('',*,*,#1485,.T.);
#1956=ORIENTED_EDGE('',*,*,#1486,.T.);
#1957=ORIENTED_EDGE('',*,*,#1482,.F.);
#1958=ORIENTED_EDGE('',*,*,#1487,.F.);
#1959=ORIENTED_EDGE('',*,*,#1488,.T.);
#1960=ORIENTED_EDGE('',*,*,#1489,.T.);
#1961=ORIENTED_EDGE('',*,*,#1485,.F.);
#1962=ORIENTED_EDGE('',*,*,#1490,.F.);
#1963=ORIENTED_EDGE('',*,*,#1491,.T.);
#1964=ORIENTED_EDGE('',*,*,#1492,.T.);
#1965=ORIENTED_EDGE('',*,*,#1488,.F.);
#1966=ORIENTED_EDGE('',*,*,#1493,.F.);
#1967=ORIENTED_EDGE('',*,*,#1494,.T.);
#1968=ORIENTED_EDGE('',*,*,#1495,.T.);
#1969=ORIENTED_EDGE('',*,*,#1491,.F.);
#1970=ORIENTED_EDGE('',*,*,#1496,.F.);
#1971=ORIENTED_EDGE('',*,*,#1497,.T.);
#1972=ORIENTED_EDGE('',*,*,#1498,.T.);
#1973=ORIENTED_EDGE('',*,*,#1494,.F.);
#1974=ORIENTED_EDGE('',*,*,#1499,.F.);
#1975=ORIENTED_EDGE('',*,*,#1500,.T.);
#1976=ORIENTED_EDGE('',*,*,#1501,.T.);
#1977=ORIENTED_EDGE('',*,*,#1497,.F.);
#1978=ORIENTED_EDGE('',*,*,#1502,.F.);
#1979=ORIENTED_EDGE('',*,*,#1503,.T.);
#1980=ORIENTED_EDGE('',*,*,#1504,.T.);
#1981=ORIENTED_EDGE('',*,*,#1500,.F.);
#1982=ORIENTED_EDGE('',*,*,#1505,.F.);
#1983=ORIENTED_EDGE('',*,*,#1506,.T.);
#1984=ORIENTED_EDGE('',*,*,#1507,.T.);
#1985=ORIENTED_EDGE('',*,*,#1503,.F.);
#1986=ORIENTED_EDGE('',*,*,#1508,.F.);
#1987=ORIENTED_EDGE('',*,*,#1509,.T.);
#1988=ORIENTED_EDGE('',*,*,#1510,.T.);
#1989=ORIENTED_EDGE('',*,*,#1506,.F.);
#1990=ORIENTED_EDGE('',*,*,#1511,.F.);
#1991=ORIENTED_EDGE('',*,*,#1512,.T.);
#1992=ORIENTED_EDGE('',*,*,#1513,.T.);
#1993=ORIENTED_EDGE('',*,*,#1509,.F.);
#1994=ORIENTED_EDGE('',*,*,#1514,.F.);
#1995=ORIENTED_EDGE('',*,*,#1515,.T.);
#1996=ORIENTED_EDGE('',*,*,#1516,.T.);
#1997=ORIENTED_EDGE('',*,*,#1512,.F.);
#1998=ORIENTED_EDGE('',*,*,#1517,.F.);
#1999=ORIENTED_EDGE('',*,*,#1518,.F.);
#2000=ORIENTED_EDGE('',*,*,#1519,.F.);
#2001=ORIENTED_EDGE('',*,*,#1520,.F.);
#2002=ORIENTED_EDGE('',*,*,#1521,.T.);
#2003=ORIENTED_EDGE('',*,*,#1522,.T.);
#2004=ORIENTED_EDGE('',*,*,#1523,.T.);
#2005=ORIENTED_EDGE('',*,*,#1524,.F.);
#2006=ORIENTED_EDGE('',*,*,#1525,.F.);
#2007=ORIENTED_EDGE('',*,*,#1526,.T.);
#2008=ORIENTED_EDGE('',*,*,#1527,.T.);
#2009=ORIENTED_EDGE('',*,*,#1522,.F.);
#2010=ORIENTED_EDGE('',*,*,#1528,.F.);
#2011=ORIENTED_EDGE('',*,*,#1529,.T.);
#2012=ORIENTED_EDGE('',*,*,#1530,.T.);
#2013=ORIENTED_EDGE('',*,*,#1526,.F.);
#2014=ORIENTED_EDGE('',*,*,#1531,.F.);
#2015=ORIENTED_EDGE('',*,*,#1532,.T.);
#2016=ORIENTED_EDGE('',*,*,#1533,.T.);
#2017=ORIENTED_EDGE('',*,*,#1529,.F.);
#2018=ORIENTED_EDGE('',*,*,#1534,.F.);
#2019=ORIENTED_EDGE('',*,*,#1535,.T.);
#2020=ORIENTED_EDGE('',*,*,#1536,.T.);
#2021=ORIENTED_EDGE('',*,*,#1532,.F.);
#2022=ORIENTED_EDGE('',*,*,#1537,.F.);
#2023=ORIENTED_EDGE('',*,*,#1538,.T.);
#2024=ORIENTED_EDGE('',*,*,#1539,.T.);
#2025=ORIENTED_EDGE('',*,*,#1535,.F.);
#2026=ORIENTED_EDGE('',*,*,#1540,.F.);
#2027=ORIENTED_EDGE('',*,*,#1541,.T.);
#2028=ORIENTED_EDGE('',*,*,#1542,.T.);
#2029=ORIENTED_EDGE('',*,*,#1538,.F.);
#2030=ORIENTED_EDGE('',*,*,#1543,.F.);
#2031=ORIENTED_EDGE('',*,*,#1544,.T.);
#2032=ORIENTED_EDGE('',*,*,#1545,.T.);
#2033=ORIENTED_EDGE('',*,*,#1541,.F.);
#2034=ORIENTED_EDGE('',*,*,#1546,.F.);
#2035=ORIENTED_EDGE('',*,*,#1547,.T.);
#2036=ORIENTED_EDGE('',*,*,#1548,.T.);
#2037=ORIENTED_EDGE('',*,*,#1544,.F.);
#2038=ORIENTED_EDGE('',*,*,#1549,.F.);
#2039=ORIENTED_EDGE('',*,*,#1550,.T.);
#2040=ORIENTED_EDGE('',*,*,#1551,.T.);
#2041=ORIENTED_EDGE('',*,*,#1547,.F.);
#2042=ORIENTED_EDGE('',*,*,#1552,.F.);
#2043=ORIENTED_EDGE('',*,*,#1553,.T.);
#2044=ORIENTED_EDGE('',*,*,#1554,.T.);
#2045=ORIENTED_EDGE('',*,*,#1550,.F.);
#2046=ORIENTED_EDGE('',*,*,#1555,.F.);
#2047=ORIENTED_EDGE('',*,*,#1556,.T.);
#2048=ORIENTED_EDGE('',*,*,#1557,.T.);
#2049=ORIENTED_EDGE('',*,*,#1553,.F.);
#2050=ORIENTED_EDGE('',*,*,#1558,.F.);
#2051=ORIENTED_EDGE('',*,*,#1559,.T.);
#2052=ORIENTED_EDGE('',*,*,#1560,.T.);
#2053=ORIENTED_EDGE('',*,*,#1556,.F.);
#2054=ORIENTED_EDGE('',*,*,#1561,.F.);
#2055=ORIENTED_EDGE('',*,*,#1562,.T.);
#2056=ORIENTED_EDGE('',*,*,#1563,.T.);
#2057=ORIENTED_EDGE('',*,*,#1559,.F.);
#2058=ORIENTED_EDGE('',*,*,#1564,.F.);
#2059=ORIENTED_EDGE('',*,*,#1565,.T.);
#2060=ORIENTED_EDGE('',*,*,#1566,.T.);
#2061=ORIENTED_EDGE('',*,*,#1562,.F.);
#2062=ORIENTED_EDGE('',*,*,#1567,.F.);
#2063=ORIENTED_EDGE('',*,*,#1568,.T.);
#2064=ORIENTED_EDGE('',*,*,#1569,.T.);
#2065=ORIENTED_EDGE('',*,*,#1565,.F.);
#2066=ORIENTED_EDGE('',*,*,#1570,.F.);
#2067=ORIENTED_EDGE('',*,*,#1571,.T.);
#2068=ORIENTED_EDGE('',*,*,#1572,.T.);
#2069=ORIENTED_EDGE('',*,*,#1568,.F.);
#2070=ORIENTED_EDGE('',*,*,#1573,.F.);
#2071=ORIENTED_EDGE('',*,*,#1574,.T.);
#2072=ORIENTED_EDGE('',*,*,#1575,.T.);
#2073=ORIENTED_EDGE('',*,*,#1571,.F.);
#2074=ORIENTED_EDGE('',*,*,#1576,.F.);
#2075=ORIENTED_EDGE('',*,*,#1577,.T.);
#2076=ORIENTED_EDGE('',*,*,#1578,.T.);
#2077=ORIENTED_EDGE('',*,*,#1574,.F.);
#2078=ORIENTED_EDGE('',*,*,#1579,.F.);
#2079=ORIENTED_EDGE('',*,*,#1580,.T.);
#2080=ORIENTED_EDGE('',*,*,#1581,.T.);
#2081=ORIENTED_EDGE('',*,*,#1577,.F.);
#2082=ORIENTED_EDGE('',*,*,#1582,.F.);
#2083=ORIENTED_EDGE('',*,*,#1583,.T.);
#2084=ORIENTED_EDGE('',*,*,#1584,.T.);
#2085=ORIENTED_EDGE('',*,*,#1580,.F.);
#2086=ORIENTED_EDGE('',*,*,#1585,.F.);
#2087=ORIENTED_EDGE('',*,*,#1586,.T.);
#2088=ORIENTED_EDGE('',*,*,#1587,.T.);
#2089=ORIENTED_EDGE('',*,*,#1583,.F.);
#2090=ORIENTED_EDGE('',*,*,#1588,.F.);
#2091=ORIENTED_EDGE('',*,*,#1589,.T.);
#2092=ORIENTED_EDGE('',*,*,#1590,.T.);
#2093=ORIENTED_EDGE('',*,*,#1586,.F.);
#2094=ORIENTED_EDGE('',*,*,#1591,.F.);
#2095=ORIENTED_EDGE('',*,*,#1592,.T.);
#2096=ORIENTED_EDGE('',*,*,#1593,.T.);
#2097=ORIENTED_EDGE('',*,*,#1589,.F.);
#2098=ORIENTED_EDGE('',*,*,#1594,.F.);
#2099=ORIENTED_EDGE('',*,*,#1595,.T.);
#2100=ORIENTED_EDGE('',*,*,#1596,.T.);
#2101=ORIENTED_EDGE('',*,*,#1592,.F.);
#2102=ORIENTED_EDGE('',*,*,#1597,.F.);
#2103=ORIENTED_EDGE('',*,*,#1598,.T.);
#2104=ORIENTED_EDGE('',*,*,#1599,.T.);
#2105=ORIENTED_EDGE('',*,*,#1595,.F.);
#2106=ORIENTED_EDGE('',*,*,#1600,.F.);
#2107=ORIENTED_EDGE('',*,*,#1601,.T.);
#2108=ORIENTED_EDGE('',*,*,#1602,.T.);
#2109=ORIENTED_EDGE('',*,*,#1598,.F.);
#2110=ORIENTED_EDGE('',*,*,#1603,.F.);
#2111=ORIENTED_EDGE('',*,*,#1604,.T.);
#2112=ORIENTED_EDGE('',*,*,#1605,.T.);
#2113=ORIENTED_EDGE('',*,*,#1601,.F.);
#2114=ORIENTED_EDGE('',*,*,#1606,.F.);
#2115=ORIENTED_EDGE('',*,*,#1607,.T.);
#2116=ORIENTED_EDGE('',*,*,#1608,.T.);
#2117=ORIENTED_EDGE('',*,*,#1604,.F.);
#2118=ORIENTED_EDGE('',*,*,#1609,.F.);
#2119=ORIENTED_EDGE('',*,*,#1610,.T.);
#2120=ORIENTED_EDGE('',*,*,#1611,.T.);
#2121=ORIENTED_EDGE('',*,*,#1607,.F.);
#2122=ORIENTED_EDGE('',*,*,#1612,.F.);
#2123=ORIENTED_EDGE('',*,*,#1613,.T.);
#2124=ORIENTED_EDGE('',*,*,#1614,.T.);
#2125=ORIENTED_EDGE('',*,*,#1610,.F.);
#2126=ORIENTED_EDGE('',*,*,#1615,.F.);
#2127=ORIENTED_EDGE('',*,*,#1616,.T.);
#2128=ORIENTED_EDGE('',*,*,#1617,.T.);
#2129=ORIENTED_EDGE('',*,*,#1613,.F.);
#2130=ORIENTED_EDGE('',*,*,#1618,.F.);
#2131=ORIENTED_EDGE('',*,*,#1619,.T.);
#2132=ORIENTED_EDGE('',*,*,#1620,.T.);
#2133=ORIENTED_EDGE('',*,*,#1616,.F.);
#2134=ORIENTED_EDGE('',*,*,#1621,.F.);
#2135=ORIENTED_EDGE('',*,*,#1622,.T.);
#2136=ORIENTED_EDGE('',*,*,#1623,.T.);
#2137=ORIENTED_EDGE('',*,*,#1619,.F.);
#2138=ORIENTED_EDGE('',*,*,#1624,.F.);
#2139=ORIENTED_EDGE('',*,*,#1625,.T.);
#2140=ORIENTED_EDGE('',*,*,#1626,.T.);
#2141=ORIENTED_EDGE('',*,*,#1622,.F.);
#2142=ORIENTED_EDGE('',*,*,#1627,.F.);
#2143=ORIENTED_EDGE('',*,*,#1628,.T.);
#2144=ORIENTED_EDGE('',*,*,#1629,.T.);
#2145=ORIENTED_EDGE('',*,*,#1625,.F.);
#2146=ORIENTED_EDGE('',*,*,#1630,.F.);
#2147=ORIENTED_EDGE('',*,*,#1631,.T.);
#2148=ORIENTED_EDGE('',*,*,#1632,.T.);
#2149=ORIENTED_EDGE('',*,*,#1628,.F.);
#2150=ORIENTED_EDGE('',*,*,#1633,.F.);
#2151=ORIENTED_EDGE('',*,*,#1634,.T.);
#2152=ORIENTED_EDGE('',*,*,#1635,.T.);
#2153=ORIENTED_EDGE('',*,*,#1631,.F.);
#2154=ORIENTED_EDGE('',*,*,#1636,.F.);
#2155=ORIENTED_EDGE('',*,*,#1637,.T.);
#2156=ORIENTED_EDGE('',*,*,#1638,.T.);
#2157=ORIENTED_EDGE('',*,*,#1634,.F.);
#2158=ORIENTED_EDGE('',*,*,#1639,.F.);
#2159=ORIENTED_EDGE('',*,*,#1640,.T.);
#2160=ORIENTED_EDGE('',*,*,#1641,.T.);
#2161=ORIENTED_EDGE('',*,*,#1637,.F.);
#2162=ORIENTED_EDGE('',*,*,#1642,.F.);
#2163=ORIENTED_EDGE('',*,*,#1643,.T.);
#2164=ORIENTED_EDGE('',*,*,#1644,.T.);
#2165=ORIENTED_EDGE('',*,*,#1640,.F.);
#2166=ORIENTED_EDGE('',*,*,#1645,.F.);
#2167=ORIENTED_EDGE('',*,*,#1646,.T.);
#2168=ORIENTED_EDGE('',*,*,#1647,.T.);
#2169=ORIENTED_EDGE('',*,*,#1643,.F.);
#2170=ORIENTED_EDGE('',*,*,#1648,.F.);
#2171=ORIENTED_EDGE('',*,*,#1649,.T.);
#2172=ORIENTED_EDGE('',*,*,#1650,.T.);
#2173=ORIENTED_EDGE('',*,*,#1646,.F.);
#2174=ORIENTED_EDGE('',*,*,#1651,.F.);
#2175=ORIENTED_EDGE('',*,*,#1652,.T.);
#2176=ORIENTED_EDGE('',*,*,#1653,.T.);
#2177=ORIENTED_EDGE('',*,*,#1649,.F.);
#2178=ORIENTED_EDGE('',*,*,#1654,.F.);
#2179=ORIENTED_EDGE('',*,*,#1655,.T.);
#2180=ORIENTED_EDGE('',*,*,#1656,.T.);
#2181=ORIENTED_EDGE('',*,*,#1652,.F.);
#2182=ORIENTED_EDGE('',*,*,#1657,.F.);
#2183=ORIENTED_EDGE('',*,*,#1658,.T.);
#2184=ORIENTED_EDGE('',*,*,#1659,.T.);
#2185=ORIENTED_EDGE('',*,*,#1655,.F.);
#2186=ORIENTED_EDGE('',*,*,#1660,.F.);
#2187=ORIENTED_EDGE('',*,*,#1661,.T.);
#2188=ORIENTED_EDGE('',*,*,#1662,.T.);
#2189=ORIENTED_EDGE('',*,*,#1658,.F.);
#2190=ORIENTED_EDGE('',*,*,#1663,.F.);
#2191=ORIENTED_EDGE('',*,*,#1664,.T.);
#2192=ORIENTED_EDGE('',*,*,#1665,.T.);
#2193=ORIENTED_EDGE('',*,*,#1661,.F.);
#2194=ORIENTED_EDGE('',*,*,#1666,.F.);
#2195=ORIENTED_EDGE('',*,*,#1667,.T.);
#2196=ORIENTED_EDGE('',*,*,#1668,.T.);
#2197=ORIENTED_EDGE('',*,*,#1669,.T.);
#2198=ORIENTED_EDGE('',*,*,#1670,.F.);
#2199=ORIENTED_EDGE('',*,*,#1671,.F.);
#2200=ORIENTED_EDGE('',*,*,#1672,.F.);
#2201=ORIENTED_EDGE('',*,*,#1673,.T.);
#2202=ORIENTED_EDGE('',*,*,#1668,.F.);
#2203=ORIENTED_EDGE('',*,*,#1674,.T.);
#2204=ORIENTED_EDGE('',*,*,#1675,.T.);
#2205=ORIENTED_EDGE('',*,*,#1676,.T.);
#2206=ORIENTED_EDGE('',*,*,#1677,.T.);
#2207=ORIENTED_EDGE('',*,*,#1676,.F.);
#2208=ORIENTED_EDGE('',*,*,#1678,.F.);
#2209=ORIENTED_EDGE('',*,*,#1679,.F.);
#2210=ORIENTED_EDGE('',*,*,#1680,.F.);
#2211=ORIENTED_EDGE('',*,*,#1681,.F.);
#2212=ORIENTED_EDGE('',*,*,#1670,.T.);
#2213=ORIENTED_EDGE('',*,*,#1682,.T.);
#2214=ORIENTED_EDGE('',*,*,#1664,.F.);
#2215=ORIENTED_EDGE('',*,*,#1683,.F.);
#2216=ORIENTED_EDGE('',*,*,#1684,.T.);
#2217=ORIENTED_EDGE('',*,*,#1685,.F.);
#2218=ORIENTED_EDGE('',*,*,#1686,.T.);
#2219=ORIENTED_EDGE('',*,*,#1524,.T.);
#2220=ORIENTED_EDGE('',*,*,#1687,.T.);
#2221=ORIENTED_EDGE('',*,*,#1688,.T.);
#2222=ORIENTED_EDGE('',*,*,#1667,.F.);
#2223=ORIENTED_EDGE('',*,*,#1677,.F.);
#2224=ORIENTED_EDGE('',*,*,#1689,.T.);
#2225=ORIENTED_EDGE('',*,*,#1684,.F.);
#2226=ORIENTED_EDGE('',*,*,#1689,.F.);
#2227=ORIENTED_EDGE('',*,*,#1690,.T.);
#2228=ORIENTED_EDGE('',*,*,#1672,.T.);
#2229=ORIENTED_EDGE('',*,*,#1691,.T.);
#2230=ORIENTED_EDGE('',*,*,#1520,.T.);
#2231=ORIENTED_EDGE('',*,*,#1692,.T.);
#2232=ORIENTED_EDGE('',*,*,#1372,.T.);
#2233=ORIENTED_EDGE('',*,*,#1693,.T.);
#2234=ORIENTED_EDGE('',*,*,#1694,.T.);
#2235=ORIENTED_EDGE('',*,*,#1690,.F.);
#2236=ORIENTED_EDGE('',*,*,#1519,.T.);
#2237=ORIENTED_EDGE('',*,*,#1695,.T.);
#2238=ORIENTED_EDGE('',*,*,#1517,.T.);
#2239=ORIENTED_EDGE('',*,*,#1514,.T.);
#2240=ORIENTED_EDGE('',*,*,#1511,.T.);
#2241=ORIENTED_EDGE('',*,*,#1508,.T.);
#2242=ORIENTED_EDGE('',*,*,#1505,.T.);
#2243=ORIENTED_EDGE('',*,*,#1502,.T.);
#2244=ORIENTED_EDGE('',*,*,#1499,.T.);
#2245=ORIENTED_EDGE('',*,*,#1496,.T.);
#2246=ORIENTED_EDGE('',*,*,#1493,.T.);
#2247=ORIENTED_EDGE('',*,*,#1490,.T.);
#2248=ORIENTED_EDGE('',*,*,#1487,.T.);
#2249=ORIENTED_EDGE('',*,*,#1484,.T.);
#2250=ORIENTED_EDGE('',*,*,#1481,.T.);
#2251=ORIENTED_EDGE('',*,*,#1478,.T.);
#2252=ORIENTED_EDGE('',*,*,#1475,.T.);
#2253=ORIENTED_EDGE('',*,*,#1472,.T.);
#2254=ORIENTED_EDGE('',*,*,#1469,.T.);
#2255=ORIENTED_EDGE('',*,*,#1466,.T.);
#2256=ORIENTED_EDGE('',*,*,#1463,.T.);
#2257=ORIENTED_EDGE('',*,*,#1460,.T.);
#2258=ORIENTED_EDGE('',*,*,#1457,.T.);
#2259=ORIENTED_EDGE('',*,*,#1454,.T.);
#2260=ORIENTED_EDGE('',*,*,#1451,.T.);
#2261=ORIENTED_EDGE('',*,*,#1448,.T.);
#2262=ORIENTED_EDGE('',*,*,#1445,.T.);
#2263=ORIENTED_EDGE('',*,*,#1442,.T.);
#2264=ORIENTED_EDGE('',*,*,#1439,.T.);
#2265=ORIENTED_EDGE('',*,*,#1436,.T.);
#2266=ORIENTED_EDGE('',*,*,#1433,.T.);
#2267=ORIENTED_EDGE('',*,*,#1430,.T.);
#2268=ORIENTED_EDGE('',*,*,#1427,.T.);
#2269=ORIENTED_EDGE('',*,*,#1424,.T.);
#2270=ORIENTED_EDGE('',*,*,#1421,.T.);
#2271=ORIENTED_EDGE('',*,*,#1418,.T.);
#2272=ORIENTED_EDGE('',*,*,#1415,.T.);
#2273=ORIENTED_EDGE('',*,*,#1412,.T.);
#2274=ORIENTED_EDGE('',*,*,#1409,.T.);
#2275=ORIENTED_EDGE('',*,*,#1406,.T.);
#2276=ORIENTED_EDGE('',*,*,#1403,.T.);
#2277=ORIENTED_EDGE('',*,*,#1400,.T.);
#2278=ORIENTED_EDGE('',*,*,#1397,.T.);
#2279=ORIENTED_EDGE('',*,*,#1394,.T.);
#2280=ORIENTED_EDGE('',*,*,#1391,.T.);
#2281=ORIENTED_EDGE('',*,*,#1388,.T.);
#2282=ORIENTED_EDGE('',*,*,#1385,.T.);
#2283=ORIENTED_EDGE('',*,*,#1382,.T.);
#2284=ORIENTED_EDGE('',*,*,#1379,.T.);
#2285=ORIENTED_EDGE('',*,*,#1376,.T.);
#2286=ORIENTED_EDGE('',*,*,#1373,.T.);
#2287=ORIENTED_EDGE('',*,*,#1692,.F.);
#2288=ORIENTED_EDGE('',*,*,#1523,.F.);
#2289=ORIENTED_EDGE('',*,*,#1527,.F.);
#2290=ORIENTED_EDGE('',*,*,#1530,.F.);
#2291=ORIENTED_EDGE('',*,*,#1533,.F.);
#2292=ORIENTED_EDGE('',*,*,#1536,.F.);
#2293=ORIENTED_EDGE('',*,*,#1539,.F.);
#2294=ORIENTED_EDGE('',*,*,#1542,.F.);
#2295=ORIENTED_EDGE('',*,*,#1545,.F.);
#2296=ORIENTED_EDGE('',*,*,#1548,.F.);
#2297=ORIENTED_EDGE('',*,*,#1551,.F.);
#2298=ORIENTED_EDGE('',*,*,#1554,.F.);
#2299=ORIENTED_EDGE('',*,*,#1557,.F.);
#2300=ORIENTED_EDGE('',*,*,#1560,.F.);
#2301=ORIENTED_EDGE('',*,*,#1563,.F.);
#2302=ORIENTED_EDGE('',*,*,#1566,.F.);
#2303=ORIENTED_EDGE('',*,*,#1569,.F.);
#2304=ORIENTED_EDGE('',*,*,#1572,.F.);
#2305=ORIENTED_EDGE('',*,*,#1575,.F.);
#2306=ORIENTED_EDGE('',*,*,#1578,.F.);
#2307=ORIENTED_EDGE('',*,*,#1581,.F.);
#2308=ORIENTED_EDGE('',*,*,#1584,.F.);
#2309=ORIENTED_EDGE('',*,*,#1587,.F.);
#2310=ORIENTED_EDGE('',*,*,#1590,.F.);
#2311=ORIENTED_EDGE('',*,*,#1593,.F.);
#2312=ORIENTED_EDGE('',*,*,#1596,.F.);
#2313=ORIENTED_EDGE('',*,*,#1599,.F.);
#2314=ORIENTED_EDGE('',*,*,#1602,.F.);
#2315=ORIENTED_EDGE('',*,*,#1605,.F.);
#2316=ORIENTED_EDGE('',*,*,#1608,.F.);
#2317=ORIENTED_EDGE('',*,*,#1611,.F.);
#2318=ORIENTED_EDGE('',*,*,#1614,.F.);
#2319=ORIENTED_EDGE('',*,*,#1617,.F.);
#2320=ORIENTED_EDGE('',*,*,#1620,.F.);
#2321=ORIENTED_EDGE('',*,*,#1623,.F.);
#2322=ORIENTED_EDGE('',*,*,#1626,.F.);
#2323=ORIENTED_EDGE('',*,*,#1629,.F.);
#2324=ORIENTED_EDGE('',*,*,#1632,.F.);
#2325=ORIENTED_EDGE('',*,*,#1635,.F.);
#2326=ORIENTED_EDGE('',*,*,#1638,.F.);
#2327=ORIENTED_EDGE('',*,*,#1641,.F.);
#2328=ORIENTED_EDGE('',*,*,#1644,.F.);
#2329=ORIENTED_EDGE('',*,*,#1647,.F.);
#2330=ORIENTED_EDGE('',*,*,#1650,.F.);
#2331=ORIENTED_EDGE('',*,*,#1653,.F.);
#2332=ORIENTED_EDGE('',*,*,#1656,.F.);
#2333=ORIENTED_EDGE('',*,*,#1659,.F.);
#2334=ORIENTED_EDGE('',*,*,#1662,.F.);
#2335=ORIENTED_EDGE('',*,*,#1665,.F.);
#2336=ORIENTED_EDGE('',*,*,#1682,.F.);
#2337=ORIENTED_EDGE('',*,*,#1669,.F.);
#2338=ORIENTED_EDGE('',*,*,#1673,.F.);
#2339=ORIENTED_EDGE('',*,*,#1518,.T.);
#2340=ORIENTED_EDGE('',*,*,#1696,.T.);
#2341=ORIENTED_EDGE('',*,*,#1515,.F.);
#2342=ORIENTED_EDGE('',*,*,#1695,.F.);
#2343=ORIENTED_EDGE('',*,*,#1691,.F.);
#2344=ORIENTED_EDGE('',*,*,#1671,.T.);
#2345=ORIENTED_EDGE('',*,*,#1683,.T.);
#2346=ORIENTED_EDGE('',*,*,#1666,.T.);
#2347=ORIENTED_EDGE('',*,*,#1663,.T.);
#2348=ORIENTED_EDGE('',*,*,#1660,.T.);
#2349=ORIENTED_EDGE('',*,*,#1657,.T.);
#2350=ORIENTED_EDGE('',*,*,#1654,.T.);
#2351=ORIENTED_EDGE('',*,*,#1651,.T.);
#2352=ORIENTED_EDGE('',*,*,#1648,.T.);
#2353=ORIENTED_EDGE('',*,*,#1645,.T.);
#2354=ORIENTED_EDGE('',*,*,#1642,.T.);
#2355=ORIENTED_EDGE('',*,*,#1639,.T.);
#2356=ORIENTED_EDGE('',*,*,#1636,.T.);
#2357=ORIENTED_EDGE('',*,*,#1633,.T.);
#2358=ORIENTED_EDGE('',*,*,#1630,.T.);
#2359=ORIENTED_EDGE('',*,*,#1627,.T.);
#2360=ORIENTED_EDGE('',*,*,#1624,.T.);
#2361=ORIENTED_EDGE('',*,*,#1621,.T.);
#2362=ORIENTED_EDGE('',*,*,#1618,.T.);
#2363=ORIENTED_EDGE('',*,*,#1615,.T.);
#2364=ORIENTED_EDGE('',*,*,#1612,.T.);
#2365=ORIENTED_EDGE('',*,*,#1609,.T.);
#2366=ORIENTED_EDGE('',*,*,#1606,.T.);
#2367=ORIENTED_EDGE('',*,*,#1603,.T.);
#2368=ORIENTED_EDGE('',*,*,#1600,.T.);
#2369=ORIENTED_EDGE('',*,*,#1597,.T.);
#2370=ORIENTED_EDGE('',*,*,#1594,.T.);
#2371=ORIENTED_EDGE('',*,*,#1591,.T.);
#2372=ORIENTED_EDGE('',*,*,#1588,.T.);
#2373=ORIENTED_EDGE('',*,*,#1585,.T.);
#2374=ORIENTED_EDGE('',*,*,#1582,.T.);
#2375=ORIENTED_EDGE('',*,*,#1579,.T.);
#2376=ORIENTED_EDGE('',*,*,#1576,.T.);
#2377=ORIENTED_EDGE('',*,*,#1573,.T.);
#2378=ORIENTED_EDGE('',*,*,#1570,.T.);
#2379=ORIENTED_EDGE('',*,*,#1567,.T.);
#2380=ORIENTED_EDGE('',*,*,#1564,.T.);
#2381=ORIENTED_EDGE('',*,*,#1561,.T.);
#2382=ORIENTED_EDGE('',*,*,#1558,.T.);
#2383=ORIENTED_EDGE('',*,*,#1555,.T.);
#2384=ORIENTED_EDGE('',*,*,#1552,.T.);
#2385=ORIENTED_EDGE('',*,*,#1549,.T.);
#2386=ORIENTED_EDGE('',*,*,#1546,.T.);
#2387=ORIENTED_EDGE('',*,*,#1543,.T.);
#2388=ORIENTED_EDGE('',*,*,#1540,.T.);
#2389=ORIENTED_EDGE('',*,*,#1537,.T.);
#2390=ORIENTED_EDGE('',*,*,#1534,.T.);
#2391=ORIENTED_EDGE('',*,*,#1531,.T.);
#2392=ORIENTED_EDGE('',*,*,#1528,.T.);
#2393=ORIENTED_EDGE('',*,*,#1525,.T.);
#2394=ORIENTED_EDGE('',*,*,#1697,.T.);
#2395=ORIENTED_EDGE('',*,*,#1693,.F.);
#2396=ORIENTED_EDGE('',*,*,#1371,.F.);
#2397=ORIENTED_EDGE('',*,*,#1375,.F.);
#2398=ORIENTED_EDGE('',*,*,#1378,.F.);
#2399=ORIENTED_EDGE('',*,*,#1381,.F.);
#2400=ORIENTED_EDGE('',*,*,#1384,.F.);
#2401=ORIENTED_EDGE('',*,*,#1387,.F.);
#2402=ORIENTED_EDGE('',*,*,#1390,.F.);
#2403=ORIENTED_EDGE('',*,*,#1393,.F.);
#2404=ORIENTED_EDGE('',*,*,#1396,.F.);
#2405=ORIENTED_EDGE('',*,*,#1399,.F.);
#2406=ORIENTED_EDGE('',*,*,#1402,.F.);
#2407=ORIENTED_EDGE('',*,*,#1405,.F.);
#2408=ORIENTED_EDGE('',*,*,#1408,.F.);
#2409=ORIENTED_EDGE('',*,*,#1411,.F.);
#2410=ORIENTED_EDGE('',*,*,#1414,.F.);
#2411=ORIENTED_EDGE('',*,*,#1417,.F.);
#2412=ORIENTED_EDGE('',*,*,#1420,.F.);
#2413=ORIENTED_EDGE('',*,*,#1423,.F.);
#2414=ORIENTED_EDGE('',*,*,#1426,.F.);
#2415=ORIENTED_EDGE('',*,*,#1429,.F.);
#2416=ORIENTED_EDGE('',*,*,#1432,.F.);
#2417=ORIENTED_EDGE('',*,*,#1435,.F.);
#2418=ORIENTED_EDGE('',*,*,#1438,.F.);
#2419=ORIENTED_EDGE('',*,*,#1441,.F.);
#2420=ORIENTED_EDGE('',*,*,#1444,.F.);
#2421=ORIENTED_EDGE('',*,*,#1447,.F.);
#2422=ORIENTED_EDGE('',*,*,#1450,.F.);
#2423=ORIENTED_EDGE('',*,*,#1453,.F.);
#2424=ORIENTED_EDGE('',*,*,#1456,.F.);
#2425=ORIENTED_EDGE('',*,*,#1459,.F.);
#2426=ORIENTED_EDGE('',*,*,#1462,.F.);
#2427=ORIENTED_EDGE('',*,*,#1465,.F.);
#2428=ORIENTED_EDGE('',*,*,#1468,.F.);
#2429=ORIENTED_EDGE('',*,*,#1471,.F.);
#2430=ORIENTED_EDGE('',*,*,#1474,.F.);
#2431=ORIENTED_EDGE('',*,*,#1477,.F.);
#2432=ORIENTED_EDGE('',*,*,#1480,.F.);
#2433=ORIENTED_EDGE('',*,*,#1483,.F.);
#2434=ORIENTED_EDGE('',*,*,#1486,.F.);
#2435=ORIENTED_EDGE('',*,*,#1489,.F.);
#2436=ORIENTED_EDGE('',*,*,#1492,.F.);
#2437=ORIENTED_EDGE('',*,*,#1495,.F.);
#2438=ORIENTED_EDGE('',*,*,#1498,.F.);
#2439=ORIENTED_EDGE('',*,*,#1501,.F.);
#2440=ORIENTED_EDGE('',*,*,#1504,.F.);
#2441=ORIENTED_EDGE('',*,*,#1507,.F.);
#2442=ORIENTED_EDGE('',*,*,#1510,.F.);
#2443=ORIENTED_EDGE('',*,*,#1513,.F.);
#2444=ORIENTED_EDGE('',*,*,#1516,.F.);
#2445=ORIENTED_EDGE('',*,*,#1696,.F.);
#2446=ORIENTED_EDGE('',*,*,#1521,.F.);
#2447=ORIENTED_EDGE('',*,*,#1687,.F.);
#2448=ORIENTED_EDGE('',*,*,#1694,.F.);
#2449=ORIENTED_EDGE('',*,*,#1697,.F.);
#2450=ORIENTED_EDGE('',*,*,#1678,.T.);
#2451=ORIENTED_EDGE('',*,*,#1698,.T.);
#2452=ORIENTED_EDGE('',*,*,#1699,.T.);
#2453=ORIENTED_EDGE('',*,*,#1698,.F.);
#2454=ORIENTED_EDGE('',*,*,#1679,.T.);
#2455=ORIENTED_EDGE('',*,*,#1699,.F.);
#2456=ORIENTED_EDGE('',*,*,#1680,.T.);
#2457=ORIENTED_EDGE('',*,*,#1700,.T.);
#2458=ORIENTED_EDGE('',*,*,#1701,.F.);
#2459=ORIENTED_EDGE('',*,*,#1700,.F.);
#2460=ORIENTED_EDGE('',*,*,#1681,.T.);
#2461=ORIENTED_EDGE('',*,*,#1701,.T.);
#2462=ORIENTED_EDGE('',*,*,#1688,.F.);
#2463=ORIENTED_EDGE('',*,*,#1702,.T.);
#2464=ORIENTED_EDGE('',*,*,#1685,.T.);
#2465=ORIENTED_EDGE('',*,*,#1702,.F.);
#2466=ORIENTED_EDGE('',*,*,#1674,.F.);
#2467=ORIENTED_EDGE('',*,*,#1675,.F.);
#2468=ORIENTED_EDGE('',*,*,#1703,.T.);
#2469=ORIENTED_EDGE('',*,*,#1686,.F.);
#2470=ORIENTED_EDGE('',*,*,#1703,.F.);
#2471=ORIENTED_EDGE('',*,*,#1704,.T.);
#2472=ORIENTED_EDGE('',*,*,#1705,.F.);
#2473=ORIENTED_EDGE('',*,*,#1706,.T.);
#2474=ORIENTED_EDGE('',*,*,#1707,.T.);
#2475=ORIENTED_EDGE('',*,*,#1706,.F.);
#2476=ORIENTED_EDGE('',*,*,#1705,.T.);
#2477=ORIENTED_EDGE('',*,*,#1708,.F.);
#2478=ORIENTED_EDGE('',*,*,#1709,.F.);
#2479=ORIENTED_EDGE('',*,*,#1710,.T.);
#2480=ORIENTED_EDGE('',*,*,#1708,.T.);
#2481=ORIENTED_EDGE('',*,*,#1710,.F.);
#2482=ORIENTED_EDGE('',*,*,#1709,.T.);
#2483=ORIENTED_EDGE('',*,*,#1707,.F.);
#2484=ORIENTED_EDGE('',*,*,#1711,.T.);
#2485=ORIENTED_EDGE('',*,*,#1704,.F.);
#2486=ORIENTED_EDGE('',*,*,#1711,.F.);
#2487=ORIENTED_EDGE('',*,*,#1712,.F.);
#2488=ORIENTED_EDGE('',*,*,#1713,.F.);
#2489=ORIENTED_EDGE('',*,*,#1714,.T.);
#2490=ORIENTED_EDGE('',*,*,#1715,.F.);
#2491=ORIENTED_EDGE('',*,*,#1714,.F.);
#2492=ORIENTED_EDGE('',*,*,#1716,.F.);
#2493=ORIENTED_EDGE('',*,*,#1717,.T.);
#2494=ORIENTED_EDGE('',*,*,#1718,.T.);
#2495=ORIENTED_EDGE('',*,*,#1719,.F.);
#2496=ORIENTED_EDGE('',*,*,#1718,.F.);
#2497=ORIENTED_EDGE('',*,*,#1720,.T.);
#2498=ORIENTED_EDGE('',*,*,#1716,.T.);
#2499=ORIENTED_EDGE('',*,*,#1720,.F.);
#2500=ORIENTED_EDGE('',*,*,#1721,.F.);
#2501=ORIENTED_EDGE('',*,*,#1722,.F.);
#2502=ORIENTED_EDGE('',*,*,#1717,.F.);
#2503=ORIENTED_EDGE('',*,*,#1723,.T.);
#2504=ORIENTED_EDGE('',*,*,#1719,.T.);
#2505=ORIENTED_EDGE('',*,*,#1723,.F.);
#2506=ORIENTED_EDGE('',*,*,#1712,.T.);
#2507=ORIENTED_EDGE('',*,*,#1713,.T.);
#2508=ORIENTED_EDGE('',*,*,#1724,.F.);
#2509=ORIENTED_EDGE('',*,*,#1725,.T.);
#2510=ORIENTED_EDGE('',*,*,#1722,.T.);
#2511=ORIENTED_EDGE('',*,*,#1721,.T.);
#2512=ORIENTED_EDGE('',*,*,#1725,.F.);
#2513=ORIENTED_EDGE('',*,*,#1724,.T.);
#2514=ORIENTED_EDGE('',*,*,#1726,.F.);
#2515=ORIENTED_EDGE('',*,*,#1727,.F.);
#2516=ORIENTED_EDGE('',*,*,#1728,.T.);
#2517=ORIENTED_EDGE('',*,*,#1726,.T.);
#2518=ORIENTED_EDGE('',*,*,#1728,.F.);
#2519=ORIENTED_EDGE('',*,*,#1715,.T.);
#2520=ORIENTED_EDGE('',*,*,#1729,.T.);
#2521=ORIENTED_EDGE('',*,*,#1729,.F.);
#2522=ORIENTED_EDGE('',*,*,#1730,.T.);
#2523=ORIENTED_EDGE('',*,*,#1731,.T.);
#2524=ORIENTED_EDGE('',*,*,#1730,.F.);
#2525=ORIENTED_EDGE('',*,*,#1727,.T.);
#2526=ORIENTED_EDGE('',*,*,#1731,.F.);
#2527=ORIENTED_EDGE('',*,*,#1732,.T.);
#2528=ORIENTED_EDGE('',*,*,#1733,.F.);
#2529=ORIENTED_EDGE('',*,*,#1732,.F.);
#2530=ORIENTED_EDGE('',*,*,#1734,.T.);
#2531=ORIENTED_EDGE('',*,*,#1735,.F.);
#2532=ORIENTED_EDGE('',*,*,#1734,.F.);
#2533=ORIENTED_EDGE('',*,*,#1736,.F.);
#2534=ORIENTED_EDGE('',*,*,#1737,.T.);
#2535=ORIENTED_EDGE('',*,*,#1733,.T.);
#2536=ORIENTED_EDGE('',*,*,#1737,.F.);
#2537=ORIENTED_EDGE('',*,*,#1738,.F.);
#2538=ORIENTED_EDGE('',*,*,#1739,.T.);
#2539=ORIENTED_EDGE('',*,*,#1736,.T.);
#2540=ORIENTED_EDGE('',*,*,#1739,.F.);
#2541=ORIENTED_EDGE('',*,*,#1740,.T.);
#2542=ORIENTED_EDGE('',*,*,#1741,.T.);
#2543=ORIENTED_EDGE('',*,*,#1742,.F.);
#2544=ORIENTED_EDGE('',*,*,#1741,.F.);
#2545=ORIENTED_EDGE('',*,*,#1742,.T.);
#2546=ORIENTED_EDGE('',*,*,#1738,.T.);
#2547=ORIENTED_EDGE('',*,*,#1743,.T.);
#2548=ORIENTED_EDGE('',*,*,#1744,.T.);
#2549=ORIENTED_EDGE('',*,*,#1745,.F.);
#2550=ORIENTED_EDGE('',*,*,#1744,.F.);
#2551=ORIENTED_EDGE('',*,*,#1745,.T.);
#2552=ORIENTED_EDGE('',*,*,#1740,.F.);
#2553=ORIENTED_EDGE('',*,*,#1743,.F.);
#2554=ORIENTED_EDGE('',*,*,#1735,.T.);
#2555=ORIENTED_EDGE('',*,*,#1746,.T.);
#2556=ORIENTED_EDGE('',*,*,#1747,.F.);
#2557=ORIENTED_EDGE('',*,*,#1748,.T.);
#2558=ORIENTED_EDGE('',*,*,#1749,.T.);
#2559=ORIENTED_EDGE('',*,*,#1750,.T.);
#2560=ORIENTED_EDGE('',*,*,#1746,.F.);
#2561=ORIENTED_EDGE('',*,*,#1750,.F.);
#2562=ORIENTED_EDGE('',*,*,#1751,.T.);
#2563=ORIENTED_EDGE('',*,*,#1752,.T.);
#2564=ORIENTED_EDGE('',*,*,#1748,.F.);
#2565=ORIENTED_EDGE('',*,*,#1749,.F.);
#2566=ORIENTED_EDGE('',*,*,#1752,.F.);
#2567=ORIENTED_EDGE('',*,*,#1747,.T.);
#2568=ORIENTED_EDGE('',*,*,#1753,.T.);
#2569=ORIENTED_EDGE('',*,*,#1754,.F.);
#2570=ORIENTED_EDGE('',*,*,#1755,.F.);
#2571=ORIENTED_EDGE('',*,*,#1753,.F.);
#2572=ORIENTED_EDGE('',*,*,#1754,.T.);
#2573=ORIENTED_EDGE('',*,*,#1755,.T.);
#2574=ORIENTED_EDGE('',*,*,#1756,.T.);
#2575=ORIENTED_EDGE('',*,*,#1757,.F.);
#2576=ORIENTED_EDGE('',*,*,#1756,.F.);
#2577=ORIENTED_EDGE('',*,*,#1757,.T.);
#2578=ORIENTED_EDGE('',*,*,#1758,.F.);
#2579=ORIENTED_EDGE('',*,*,#1759,.T.);
#2580=ORIENTED_EDGE('',*,*,#1760,.T.);
#2581=ORIENTED_EDGE('',*,*,#1761,.F.);
#2582=ORIENTED_EDGE('',*,*,#1760,.F.);
#2583=ORIENTED_EDGE('',*,*,#1762,.T.);
#2584=ORIENTED_EDGE('',*,*,#1763,.T.);
#2585=ORIENTED_EDGE('',*,*,#1764,.F.);
#2586=ORIENTED_EDGE('',*,*,#1763,.F.);
#2587=ORIENTED_EDGE('',*,*,#1759,.F.);
#2588=ORIENTED_EDGE('',*,*,#1764,.T.);
#2589=ORIENTED_EDGE('',*,*,#1762,.F.);
#2590=ORIENTED_EDGE('',*,*,#1765,.T.);
#2591=ORIENTED_EDGE('',*,*,#1765,.F.);
#2592=ORIENTED_EDGE('',*,*,#1766,.T.);
#2593=ORIENTED_EDGE('',*,*,#1758,.T.);
#2594=ORIENTED_EDGE('',*,*,#1766,.F.);
#2595=ORIENTED_EDGE('',*,*,#1751,.F.);
#2596=ORIENTED_EDGE('',*,*,#1761,.T.);
#2597=ORIENTED_EDGE('',*,*,#1767,.F.);
#2598=ORIENTED_EDGE('',*,*,#1768,.F.);
#2599=ORIENTED_EDGE('',*,*,#1769,.T.);
#2600=ORIENTED_EDGE('',*,*,#1770,.F.);
#2601=ORIENTED_EDGE('',*,*,#1769,.F.);
#2602=ORIENTED_EDGE('',*,*,#1771,.F.);
#2603=ORIENTED_EDGE('',*,*,#1772,.T.);
#2604=ORIENTED_EDGE('',*,*,#1773,.T.);
#2605=ORIENTED_EDGE('',*,*,#1774,.T.);
#2606=ORIENTED_EDGE('',*,*,#1775,.T.);
#2607=ORIENTED_EDGE('',*,*,#1776,.T.);
#2608=ORIENTED_EDGE('',*,*,#1777,.T.);
#2609=ORIENTED_EDGE('',*,*,#1778,.F.);
#2610=ORIENTED_EDGE('',*,*,#1779,.T.);
#2611=ORIENTED_EDGE('',*,*,#1780,.T.);
#2612=ORIENTED_EDGE('',*,*,#1775,.F.);
#2613=ORIENTED_EDGE('',*,*,#1779,.F.);
#2614=ORIENTED_EDGE('',*,*,#1781,.F.);
#2615=ORIENTED_EDGE('',*,*,#1767,.T.);
#2616=ORIENTED_EDGE('',*,*,#1782,.T.);
#2617=ORIENTED_EDGE('',*,*,#1770,.T.);
#2618=ORIENTED_EDGE('',*,*,#1783,.F.);
#2619=ORIENTED_EDGE('',*,*,#1772,.F.);
#2620=ORIENTED_EDGE('',*,*,#1784,.F.);
#2621=ORIENTED_EDGE('',*,*,#1785,.F.);
#2622=ORIENTED_EDGE('',*,*,#1786,.F.);
#2623=ORIENTED_EDGE('',*,*,#1787,.F.);
#2624=ORIENTED_EDGE('',*,*,#1788,.F.);
#2625=ORIENTED_EDGE('',*,*,#1777,.F.);
#2626=ORIENTED_EDGE('',*,*,#1783,.T.);
#2627=ORIENTED_EDGE('',*,*,#1789,.T.);
#2628=ORIENTED_EDGE('',*,*,#1786,.T.);
#2629=ORIENTED_EDGE('',*,*,#1776,.F.);
#2630=ORIENTED_EDGE('',*,*,#1780,.F.);
#2631=ORIENTED_EDGE('',*,*,#1782,.F.);
#2632=ORIENTED_EDGE('',*,*,#1773,.F.);
#2633=ORIENTED_EDGE('',*,*,#1784,.T.);
#2634=ORIENTED_EDGE('',*,*,#1771,.T.);
#2635=ORIENTED_EDGE('',*,*,#1768,.T.);
#2636=ORIENTED_EDGE('',*,*,#1781,.T.);
#2637=ORIENTED_EDGE('',*,*,#1778,.T.);
#2638=ORIENTED_EDGE('',*,*,#1788,.T.);
#2639=ORIENTED_EDGE('',*,*,#1790,.F.);
#2640=ORIENTED_EDGE('',*,*,#1785,.T.);
#2641=ORIENTED_EDGE('',*,*,#1790,.T.);
#2642=ORIENTED_EDGE('',*,*,#1787,.T.);
#2643=ORIENTED_EDGE('',*,*,#1789,.F.);
#2644=ORIENTED_EDGE('',*,*,#1791,.T.);
#2645=ORIENTED_EDGE('',*,*,#1792,.F.);
#2646=ORIENTED_EDGE('',*,*,#1793,.F.);
#2647=ORIENTED_EDGE('',*,*,#1794,.T.);
#2648=ORIENTED_EDGE('',*,*,#1795,.T.);
#2649=ORIENTED_EDGE('',*,*,#1796,.F.);
#2650=ORIENTED_EDGE('',*,*,#1797,.F.);
#2651=ORIENTED_EDGE('',*,*,#1792,.T.);
#2652=ORIENTED_EDGE('',*,*,#1798,.T.);
#2653=ORIENTED_EDGE('',*,*,#1799,.F.);
#2654=ORIENTED_EDGE('',*,*,#1800,.F.);
#2655=ORIENTED_EDGE('',*,*,#1796,.T.);
#2656=ORIENTED_EDGE('',*,*,#1801,.T.);
#2657=ORIENTED_EDGE('',*,*,#1794,.F.);
#2658=ORIENTED_EDGE('',*,*,#1802,.F.);
#2659=ORIENTED_EDGE('',*,*,#1799,.T.);
#2660=ORIENTED_EDGE('',*,*,#1793,.T.);
#2661=ORIENTED_EDGE('',*,*,#1797,.T.);
#2662=ORIENTED_EDGE('',*,*,#1800,.T.);
#2663=ORIENTED_EDGE('',*,*,#1802,.T.);
#2664=ORIENTED_EDGE('',*,*,#1774,.F.);
#2665=ORIENTED_EDGE('',*,*,#1791,.F.);
#2666=ORIENTED_EDGE('',*,*,#1801,.F.);
#2667=ORIENTED_EDGE('',*,*,#1798,.F.);
#2668=ORIENTED_EDGE('',*,*,#1795,.F.);
#2669=CYLINDRICAL_SURFACE('',#3040,104.958734125);
#2670=CYLINDRICAL_SURFACE('',#3041,104.958734125);
#2671=CYLINDRICAL_SURFACE('',#3042,104.958734125);
#2672=CYLINDRICAL_SURFACE('',#3043,104.958734125);
#2673=CYLINDRICAL_SURFACE('',#3044,104.958734125);
#2674=CYLINDRICAL_SURFACE('',#3045,104.958734125);
#2675=CYLINDRICAL_SURFACE('',#3046,104.958734125);
#2676=CYLINDRICAL_SURFACE('',#3047,104.958734125);
#2677=CYLINDRICAL_SURFACE('',#3048,104.958734125);
#2678=CYLINDRICAL_SURFACE('',#3049,104.958734125);
#2679=CYLINDRICAL_SURFACE('',#3050,104.958734125);
#2680=CYLINDRICAL_SURFACE('',#3051,104.958734125);
#2681=CYLINDRICAL_SURFACE('',#3052,104.958734125);
#2682=CYLINDRICAL_SURFACE('',#3053,104.958734125);
#2683=CYLINDRICAL_SURFACE('',#3054,104.958734125);
#2684=CYLINDRICAL_SURFACE('',#3055,104.958734125);
#2685=CYLINDRICAL_SURFACE('',#3056,104.958734125);
#2686=CYLINDRICAL_SURFACE('',#3057,104.958734125);
#2687=CYLINDRICAL_SURFACE('',#3058,104.958734125);
#2688=CYLINDRICAL_SURFACE('',#3059,104.958734125);
#2689=CYLINDRICAL_SURFACE('',#3060,104.958734125);
#2690=CYLINDRICAL_SURFACE('',#3061,104.958734125);
#2691=CYLINDRICAL_SURFACE('',#3062,104.958734125);
#2692=CYLINDRICAL_SURFACE('',#3063,104.958734125);
#2693=CYLINDRICAL_SURFACE('',#3064,104.958734125);
#2694=CYLINDRICAL_SURFACE('',#3065,104.958734125);
#2695=CYLINDRICAL_SURFACE('',#3066,104.958734125);
#2696=CYLINDRICAL_SURFACE('',#3067,104.958734125);
#2697=CYLINDRICAL_SURFACE('',#3068,104.958734125);
#2698=CYLINDRICAL_SURFACE('',#3069,104.958734125);
#2699=CYLINDRICAL_SURFACE('',#3070,104.958734125);
#2700=CYLINDRICAL_SURFACE('',#3071,104.958734125);
#2701=CYLINDRICAL_SURFACE('',#3072,104.958734125);
#2702=CYLINDRICAL_SURFACE('',#3073,104.958734125);
#2703=CYLINDRICAL_SURFACE('',#3074,104.958734125);
#2704=CYLINDRICAL_SURFACE('',#3075,104.958734125);
#2705=CYLINDRICAL_SURFACE('',#3076,104.958734125);
#2706=CYLINDRICAL_SURFACE('',#3077,104.958734125);
#2707=CYLINDRICAL_SURFACE('',#3078,104.958734125);
#2708=CYLINDRICAL_SURFACE('',#3079,104.958734125);
#2709=CYLINDRICAL_SURFACE('',#3080,104.958734125);
#2710=CYLINDRICAL_SURFACE('',#3081,104.958734125);
#2711=CYLINDRICAL_SURFACE('',#3082,104.958734125);
#2712=CYLINDRICAL_SURFACE('',#3083,104.958734125);
#2713=CYLINDRICAL_SURFACE('',#3084,104.958734125);
#2714=CYLINDRICAL_SURFACE('',#3085,104.958734125);
#2715=CYLINDRICAL_SURFACE('',#3086,104.958734125);
#2716=CYLINDRICAL_SURFACE('',#3087,104.958734125);
#2717=CYLINDRICAL_SURFACE('',#3088,104.958734125);
#2718=CYLINDRICAL_SURFACE('',#3089,104.958734125);
#2719=CYLINDRICAL_SURFACE('',#3090,105.5);
#2720=CYLINDRICAL_SURFACE('',#3092,105.5);
#2721=CYLINDRICAL_SURFACE('',#3093,105.5);
#2722=CYLINDRICAL_SURFACE('',#3094,105.5);
#2723=CYLINDRICAL_SURFACE('',#3095,105.5);
#2724=CYLINDRICAL_SURFACE('',#3096,105.5);
#2725=CYLINDRICAL_SURFACE('',#3097,105.5);
#2726=CYLINDRICAL_SURFACE('',#3098,105.5);
#2727=CYLINDRICAL_SURFACE('',#3099,105.5);
#2728=CYLINDRICAL_SURFACE('',#3100,105.5);
#2729=CYLINDRICAL_SURFACE('',#3101,105.5);
#2730=CYLINDRICAL_SURFACE('',#3102,105.5);
#2731=CYLINDRICAL_SURFACE('',#3103,105.5);
#2732=CYLINDRICAL_SURFACE('',#3104,105.5);
#2733=CYLINDRICAL_SURFACE('',#3105,105.5);
#2734=CYLINDRICAL_SURFACE('',#3106,105.5);
#2735=CYLINDRICAL_SURFACE('',#3107,105.5);
#2736=CYLINDRICAL_SURFACE('',#3108,105.5);
#2737=CYLINDRICAL_SURFACE('',#3109,105.5);
#2738=CYLINDRICAL_SURFACE('',#3110,105.5);
#2739=CYLINDRICAL_SURFACE('',#3111,105.5);
#2740=CYLINDRICAL_SURFACE('',#3112,105.5);
#2741=CYLINDRICAL_SURFACE('',#3113,105.5);
#2742=CYLINDRICAL_SURFACE('',#3114,105.5);
#2743=CYLINDRICAL_SURFACE('',#3115,105.5);
#2744=CYLINDRICAL_SURFACE('',#3116,105.5);
#2745=CYLINDRICAL_SURFACE('',#3117,105.5);
#2746=CYLINDRICAL_SURFACE('',#3118,105.5);
#2747=CYLINDRICAL_SURFACE('',#3119,105.5);
#2748=CYLINDRICAL_SURFACE('',#3120,105.5);
#2749=CYLINDRICAL_SURFACE('',#3121,105.5);
#2750=CYLINDRICAL_SURFACE('',#3122,105.5);
#2751=CYLINDRICAL_SURFACE('',#3123,105.5);
#2752=CYLINDRICAL_SURFACE('',#3124,105.5);
#2753=CYLINDRICAL_SURFACE('',#3125,105.5);
#2754=CYLINDRICAL_SURFACE('',#3126,105.5);
#2755=CYLINDRICAL_SURFACE('',#3127,105.5);
#2756=CYLINDRICAL_SURFACE('',#3128,105.5);
#2757=CYLINDRICAL_SURFACE('',#3129,105.5);
#2758=CYLINDRICAL_SURFACE('',#3130,105.5);
#2759=CYLINDRICAL_SURFACE('',#3131,105.5);
#2760=CYLINDRICAL_SURFACE('',#3132,105.5);
#2761=CYLINDRICAL_SURFACE('',#3133,105.5);
#2762=CYLINDRICAL_SURFACE('',#3134,105.5);
#2763=CYLINDRICAL_SURFACE('',#3135,105.5);
#2764=CYLINDRICAL_SURFACE('',#3136,105.5);
#2765=CYLINDRICAL_SURFACE('',#3137,105.5);
#2766=CYLINDRICAL_SURFACE('',#3138,105.5);
#2767=CYLINDRICAL_SURFACE('',#3139,105.5);
#2768=CYLINDRICAL_SURFACE('',#3141,120.5);
#2769=CYLINDRICAL_SURFACE('',#3145,105.5);
#2770=CYLINDRICAL_SURFACE('',#3157,104.958734125);
#2771=CYLINDRICAL_SURFACE('',#3158,105.5);
#2772=CYLINDRICAL_SURFACE('',#3159,9.99999999999999);
#2773=CYLINDRICAL_SURFACE('',#3162,9.99999999999999);
#2774=CYLINDRICAL_SURFACE('',#3170,15.);
#2775=CYLINDRICAL_SURFACE('',#3175,9.99999999999999);
#2776=CYLINDRICAL_SURFACE('',#3183,12.5);
#2777=CYLINDRICAL_SURFACE('',#3191,15.);
#2778=CYLINDRICAL_SURFACE('',#3192,14.);
#2779=CYLINDRICAL_SURFACE('',#3193,13.5);
#2780=CYLINDRICAL_SURFACE('',#3197,12.5);
#2781=CYLINDRICAL_SURFACE('',#3201,11.5);
#2782=CYLINDRICAL_SURFACE('',#3212,50.);
#2783=CYLINDRICAL_SURFACE('',#3214,52.);
#2784=CYLINDRICAL_SURFACE('',#3218,56.);
#2785=CYLINDRICAL_SURFACE('',#3231,15.);
#2786=CYLINDRICAL_SURFACE('',#3237,14.);
#2787=CYLINDRICAL_SURFACE('',#3241,12.5);
#2788=CYLINDRICAL_SURFACE('',#3244,11.5);
#2789=CYLINDRICAL_SURFACE('',#3250,11.);
#2790=CYLINDRICAL_SURFACE('',#3253,7.5);
#2791=CYLINDRICAL_SURFACE('',#3256,7.5);
#2792=CYLINDRICAL_SURFACE('',#3259,7.5);
#2793=CYLINDRICAL_SURFACE('',#3263,25.);
#2794=ADVANCED_FACE('',(#207),#2669,.F.);
#2795=ADVANCED_FACE('',(#208),#2670,.F.);
#2796=ADVANCED_FACE('',(#209),#2671,.F.);
#2797=ADVANCED_FACE('',(#210),#2672,.F.);
#2798=ADVANCED_FACE('',(#211),#2673,.F.);
#2799=ADVANCED_FACE('',(#212),#2674,.F.);
#2800=ADVANCED_FACE('',(#213),#2675,.F.);
#2801=ADVANCED_FACE('',(#214),#2676,.F.);
#2802=ADVANCED_FACE('',(#215),#2677,.F.);
#2803=ADVANCED_FACE('',(#216),#2678,.F.);
#2804=ADVANCED_FACE('',(#217),#2679,.F.);
#2805=ADVANCED_FACE('',(#218),#2680,.F.);
#2806=ADVANCED_FACE('',(#219),#2681,.F.);
#2807=ADVANCED_FACE('',(#220),#2682,.F.);
#2808=ADVANCED_FACE('',(#221),#2683,.F.);
#2809=ADVANCED_FACE('',(#222),#2684,.F.);
#2810=ADVANCED_FACE('',(#223),#2685,.F.);
#2811=ADVANCED_FACE('',(#224),#2686,.F.);
#2812=ADVANCED_FACE('',(#225),#2687,.F.);
#2813=ADVANCED_FACE('',(#226),#2688,.F.);
#2814=ADVANCED_FACE('',(#227),#2689,.F.);
#2815=ADVANCED_FACE('',(#228),#2690,.F.);
#2816=ADVANCED_FACE('',(#229),#2691,.F.);
#2817=ADVANCED_FACE('',(#230),#2692,.F.);
#2818=ADVANCED_FACE('',(#231),#2693,.F.);
#2819=ADVANCED_FACE('',(#232),#2694,.F.);
#2820=ADVANCED_FACE('',(#233),#2695,.F.);
#2821=ADVANCED_FACE('',(#234),#2696,.F.);
#2822=ADVANCED_FACE('',(#235),#2697,.F.);
#2823=ADVANCED_FACE('',(#236),#2698,.F.);
#2824=ADVANCED_FACE('',(#237),#2699,.F.);
#2825=ADVANCED_FACE('',(#238),#2700,.F.);
#2826=ADVANCED_FACE('',(#239),#2701,.F.);
#2827=ADVANCED_FACE('',(#240),#2702,.F.);
#2828=ADVANCED_FACE('',(#241),#2703,.F.);
#2829=ADVANCED_FACE('',(#242),#2704,.F.);
#2830=ADVANCED_FACE('',(#243),#2705,.F.);
#2831=ADVANCED_FACE('',(#244),#2706,.F.);
#2832=ADVANCED_FACE('',(#245),#2707,.F.);
#2833=ADVANCED_FACE('',(#246),#2708,.F.);
#2834=ADVANCED_FACE('',(#247),#2709,.F.);
#2835=ADVANCED_FACE('',(#248),#2710,.F.);
#2836=ADVANCED_FACE('',(#249),#2711,.F.);
#2837=ADVANCED_FACE('',(#250),#2712,.F.);
#2838=ADVANCED_FACE('',(#251),#2713,.F.);
#2839=ADVANCED_FACE('',(#252),#2714,.F.);
#2840=ADVANCED_FACE('',(#253),#2715,.F.);
#2841=ADVANCED_FACE('',(#254),#2716,.F.);
#2842=ADVANCED_FACE('',(#255),#2717,.F.);
#2843=ADVANCED_FACE('',(#256),#2718,.F.);
#2844=ADVANCED_FACE('',(#257),#2719,.F.);
#2845=ADVANCED_FACE('',(#258),#2720,.F.);
#2846=ADVANCED_FACE('',(#259),#2721,.F.);
#2847=ADVANCED_FACE('',(#260),#2722,.F.);
#2848=ADVANCED_FACE('',(#261),#2723,.F.);
#2849=ADVANCED_FACE('',(#262),#2724,.F.);
#2850=ADVANCED_FACE('',(#263),#2725,.F.);
#2851=ADVANCED_FACE('',(#264),#2726,.F.);
#2852=ADVANCED_FACE('',(#265),#2727,.F.);
#2853=ADVANCED_FACE('',(#266),#2728,.F.);
#2854=ADVANCED_FACE('',(#267),#2729,.F.);
#2855=ADVANCED_FACE('',(#268),#2730,.F.);
#2856=ADVANCED_FACE('',(#269),#2731,.F.);
#2857=ADVANCED_FACE('',(#270),#2732,.F.);
#2858=ADVANCED_FACE('',(#271),#2733,.F.);
#2859=ADVANCED_FACE('',(#272),#2734,.F.);
#2860=ADVANCED_FACE('',(#273),#2735,.F.);
#2861=ADVANCED_FACE('',(#274),#2736,.F.);
#2862=ADVANCED_FACE('',(#275),#2737,.F.);
#2863=ADVANCED_FACE('',(#276),#2738,.F.);
#2864=ADVANCED_FACE('',(#277),#2739,.F.);
#2865=ADVANCED_FACE('',(#278),#2740,.F.);
#2866=ADVANCED_FACE('',(#279),#2741,.F.);
#2867=ADVANCED_FACE('',(#280),#2742,.F.);
#2868=ADVANCED_FACE('',(#281),#2743,.F.);
#2869=ADVANCED_FACE('',(#282),#2744,.F.);
#2870=ADVANCED_FACE('',(#283),#2745,.F.);
#2871=ADVANCED_FACE('',(#284),#2746,.F.);
#2872=ADVANCED_FACE('',(#285),#2747,.F.);
#2873=ADVANCED_FACE('',(#286),#2748,.F.);
#2874=ADVANCED_FACE('',(#287),#2749,.F.);
#2875=ADVANCED_FACE('',(#288),#2750,.F.);
#2876=ADVANCED_FACE('',(#289),#2751,.F.);
#2877=ADVANCED_FACE('',(#290),#2752,.F.);
#2878=ADVANCED_FACE('',(#291),#2753,.F.);
#2879=ADVANCED_FACE('',(#292),#2754,.F.);
#2880=ADVANCED_FACE('',(#293),#2755,.F.);
#2881=ADVANCED_FACE('',(#294),#2756,.F.);
#2882=ADVANCED_FACE('',(#295),#2757,.F.);
#2883=ADVANCED_FACE('',(#296),#2758,.F.);
#2884=ADVANCED_FACE('',(#297),#2759,.F.);
#2885=ADVANCED_FACE('',(#298),#2760,.F.);
#2886=ADVANCED_FACE('',(#299),#2761,.F.);
#2887=ADVANCED_FACE('',(#300),#2762,.F.);
#2888=ADVANCED_FACE('',(#301),#2763,.F.);
#2889=ADVANCED_FACE('',(#302),#2764,.F.);
#2890=ADVANCED_FACE('',(#303),#2765,.F.);
#2891=ADVANCED_FACE('',(#304),#2766,.F.);
#2892=ADVANCED_FACE('',(#305),#2767,.F.);
#2893=ADVANCED_FACE('',(#306,#112,#113),#2768,.T.);
#2894=ADVANCED_FACE('',(#307),#2769,.F.);
#2895=ADVANCED_FACE('',(#308,#114),#80,.T.);
#2896=ADVANCED_FACE('',(#309,#115),#81,.F.);
#2897=ADVANCED_FACE('',(#310,#116),#82,.T.);
#2898=ADVANCED_FACE('',(#311),#74,.T.);
#2899=ADVANCED_FACE('',(#312),#83,.T.);
#2900=ADVANCED_FACE('',(#313),#84,.T.);
#2901=ADVANCED_FACE('',(#314),#69,.F.);
#2902=ADVANCED_FACE('',(#315),#2770,.F.);
#2903=ADVANCED_FACE('',(#316),#70,.F.);
#2904=ADVANCED_FACE('',(#317),#2771,.T.);
#2905=ADVANCED_FACE('',(#318),#2772,.F.);
#2906=ADVANCED_FACE('',(#319),#85,.T.);
#2907=ADVANCED_FACE('',(#320),#2773,.F.);
#2908=ADVANCED_FACE('',(#321),#86,.T.);
#2909=ADVANCED_FACE('',(#322),#75,.F.);
#2910=ADVANCED_FACE('',(#323),#76,.T.);
#2911=ADVANCED_FACE('',(#324),#87,.F.);
#2912=ADVANCED_FACE('',(#325),#2774,.T.);
#2913=ADVANCED_FACE('',(#326,#117),#88,.F.);
#2914=ADVANCED_FACE('',(#327),#2775,.T.);
#2915=ADVANCED_FACE('',(#328),#89,.F.);
#2916=ADVANCED_FACE('',(#329),#77,.T.);
#2917=ADVANCED_FACE('',(#330),#2776,.F.);
#2918=ADVANCED_FACE('',(#331,#118),#90,.F.);
#2919=ADVANCED_FACE('',(#332,#119),#91,.T.);
#2920=ADVANCED_FACE('',(#333,#120),#2777,.T.);
#2921=ADVANCED_FACE('',(#334,#121),#2778,.F.);
#2922=ADVANCED_FACE('',(#335),#2779,.T.);
#2923=ADVANCED_FACE('',(#336,#122),#92,.T.);
#2924=ADVANCED_FACE('',(#337),#2780,.T.);
#2925=ADVANCED_FACE('',(#338,#123),#93,.F.);
#2926=ADVANCED_FACE('',(#339),#2781,.F.);
#2927=ADVANCED_FACE('',(#340,#124),#94,.T.);
#2928=ADVANCED_FACE('',(#341,#125),#95,.F.);
#2929=ADVANCED_FACE('',(#342),#78,.T.);
#2930=ADVANCED_FACE('',(#343),#79,.F.);
#2931=ADVANCED_FACE('',(#344),#2782,.F.);
#2932=ADVANCED_FACE('',(#345),#2783,.T.);
#2933=ADVANCED_FACE('',(#346,#126),#96,.T.);
#2934=ADVANCED_FACE('',(#347),#2784,.T.);
#2935=ADVANCED_FACE('',(#348,#127),#97,.T.);
#2936=ADVANCED_FACE('',(#349,#128),#98,.F.);
#2937=ADVANCED_FACE('',(#350,#129),#99,.T.);
#2938=ADVANCED_FACE('',(#351),#11,.T.);
#2939=ADVANCED_FACE('',(#352),#2785,.T.);
#2940=ADVANCED_FACE('',(#353),#12,.F.);
#2941=ADVANCED_FACE('',(#354),#2786,.F.);
#2942=ADVANCED_FACE('',(#355,#130),#100,.T.);
#2943=ADVANCED_FACE('',(#356),#2787,.T.);
#2944=ADVANCED_FACE('',(#357),#2788,.F.);
#2945=ADVANCED_FACE('',(#358,#131),#101,.F.);
#2946=ADVANCED_FACE('',(#359,#132),#102,.F.);
#2947=ADVANCED_FACE('',(#360),#2789,.F.);
#2948=ADVANCED_FACE('',(#361,#133),#103,.F.);
#2949=ADVANCED_FACE('',(#362),#2790,.T.);
#2950=ADVANCED_FACE('',(#363),#2791,.T.);
#2951=ADVANCED_FACE('',(#364),#2792,.T.);
#2952=ADVANCED_FACE('',(#365),#104,.T.);
#2953=ADVANCED_FACE('',(#366),#105,.F.);
#2954=ADVANCED_FACE('',(#367),#106,.F.);
#2955=ADVANCED_FACE('',(#368),#71,.T.);
#2956=ADVANCED_FACE('',(#369),#72,.T.);
#2957=ADVANCED_FACE('',(#370),#73,.T.);
#2958=ADVANCED_FACE('',(#371),#2793,.T.);
#2959=ADVANCED_FACE('',(#372),#107,.F.);
#2960=ADVANCED_FACE('',(#373),#108,.F.);
#2961=ADVANCED_FACE('',(#374),#109,.F.);
#2962=ADVANCED_FACE('',(#375,#134),#110,.T.);
#2963=ADVANCED_FACE('',(#376),#111,.F.);
#2964=CLOSED_SHELL('',(#2794,#2795,#2796,#2797,#2798,#2799,#2800,#2801,
#2802,#2803,#2804,#2805,#2806,#2807,#2808,#2809,#2810,#2811,#2812,#2813,
#2814,#2815,#2816,#2817,#2818,#2819,#2820,#2821,#2822,#2823,#2824,#2825,
#2826,#2827,#2828,#2829,#2830,#2831,#2832,#2833,#2834,#2835,#2836,#2837,
#2838,#2839,#2840,#2841,#2842,#2843,#2844,#2845,#2846,#2847,#2848,#2849,
#2850,#2851,#2852,#2853,#2854,#2855,#2856,#2857,#2858,#2859,#2860,#2861,
#2862,#2863,#2864,#2865,#2866,#2867,#2868,#2869,#2870,#2871,#2872,#2873,
#2874,#2875,#2876,#2877,#2878,#2879,#2880,#2881,#2882,#2883,#2884,#2885,
#2886,#2887,#2888,#2889,#2890,#2891,#2892,#2893,#2894,#2895,#2896,#2897,
#2898,#2899,#2900,#2901,#2902,#2903,#2904,#2905,#2906,#2907,#2908,#2909,
#2910));
#2965=CLOSED_SHELL('',(#2911,#2912,#2913,#2914,#2915,#2916));
#2966=CLOSED_SHELL('',(#2917,#2918,#2919,#2920,#2921,#2922,#2923,#2924,
#2925,#2926,#2927));
#2967=CLOSED_SHELL('',(#2928,#2929,#2930,#2931,#2932,#2933,#2934,#2935,
#2936));
#2968=CLOSED_SHELL('',(#2937,#2938,#2939,#2940,#2941,#2942,#2943,#2944,
#2945,#2946,#2947,#2948));
#2969=CLOSED_SHELL('',(#2949,#2950,#2951,#2952,#2953,#2954,#2955,#2956,
#2957,#2958,#2959,#2960,#2961,#2962,#2963));
#2970=DERIVED_UNIT_ELEMENT(#2982,1.);
#2971=DERIVED_UNIT_ELEMENT(#13596,-3.);
#2972=DERIVED_UNIT_ELEMENT(#2982,1.);
#2973=DERIVED_UNIT_ELEMENT(#13596,-3.);
#2974=DERIVED_UNIT_ELEMENT(#2982,1.);
#2975=DERIVED_UNIT_ELEMENT(#13596,-3.);
#2976=DERIVED_UNIT_ELEMENT(#2982,1.);
#2977=DERIVED_UNIT_ELEMENT(#13596,-3.);
#2978=DERIVED_UNIT_ELEMENT(#2982,1.);
#2979=DERIVED_UNIT_ELEMENT(#13596,-3.);
#2980=DERIVED_UNIT_ELEMENT(#2982,1.);
#2981=DERIVED_UNIT_ELEMENT(#13596,-3.);
#2982=(
MASS_UNIT()
NAMED_UNIT(*)
SI_UNIT(.KILO.,.GRAM.)
);
#2983=DERIVED_UNIT((#2970,#2971));
#2984=DERIVED_UNIT((#2972,#2973));
#2985=DERIVED_UNIT((#2974,#2975));
#2986=DERIVED_UNIT((#2976,#2977));
#2987=DERIVED_UNIT((#2978,#2979));
#2988=DERIVED_UNIT((#2980,#2981));
#2989=MEASURE_REPRESENTATION_ITEM('density measure',
POSITIVE_RATIO_MEASURE(7850.),#2983);
#2990=MEASURE_REPRESENTATION_ITEM('density measure',
POSITIVE_RATIO_MEASURE(7850.),#2984);
#2991=MEASURE_REPRESENTATION_ITEM('density measure',
POSITIVE_RATIO_MEASURE(7850.),#2985);
#2992=MEASURE_REPRESENTATION_ITEM('density measure',
POSITIVE_RATIO_MEASURE(7850.),#2986);
#2993=MEASURE_REPRESENTATION_ITEM('density measure',
POSITIVE_RATIO_MEASURE(7850.),#2987);
#2994=MEASURE_REPRESENTATION_ITEM('density measure',
POSITIVE_RATIO_MEASURE(7850.),#2988);
#2995=PROPERTY_DEFINITION_REPRESENTATION(#3025,#3007);
#2996=PROPERTY_DEFINITION_REPRESENTATION(#3026,#3008);
#2997=PROPERTY_DEFINITION_REPRESENTATION(#3027,#3009);
#2998=PROPERTY_DEFINITION_REPRESENTATION(#3028,#3010);
#2999=PROPERTY_DEFINITION_REPRESENTATION(#3029,#3011);
#3000=PROPERTY_DEFINITION_REPRESENTATION(#3030,#3012);
#3001=PROPERTY_DEFINITION_REPRESENTATION(#3031,#3013);
#3002=PROPERTY_DEFINITION_REPRESENTATION(#3032,#3014);
#3003=PROPERTY_DEFINITION_REPRESENTATION(#3033,#3015);
#3004=PROPERTY_DEFINITION_REPRESENTATION(#3034,#3016);
#3005=PROPERTY_DEFINITION_REPRESENTATION(#3035,#3017);
#3006=PROPERTY_DEFINITION_REPRESENTATION(#3036,#3018);
#3007=REPRESENTATION('material name',(#3019),#13588);
#3008=REPRESENTATION('density',(#2989),#13588);
#3009=REPRESENTATION('material name',(#3020),#13589);
#3010=REPRESENTATION('density',(#2990),#13589);
#3011=REPRESENTATION('material name',(#3021),#13590);
#3012=REPRESENTATION('density',(#2991),#13590);
#3013=REPRESENTATION('material name',(#3022),#13591);
#3014=REPRESENTATION('density',(#2992),#13591);
#3015=REPRESENTATION('material name',(#3023),#13592);
#3016=REPRESENTATION('density',(#2993),#13592);
#3017=REPRESENTATION('material name',(#3024),#13593);
#3018=REPRESENTATION('density',(#2994),#13593);
#3019=DESCRIPTIVE_REPRESENTATION_ITEM('Steel','Steel');
#3020=DESCRIPTIVE_REPRESENTATION_ITEM('Steel','Steel');
#3021=DESCRIPTIVE_REPRESENTATION_ITEM('Steel','Steel');
#3022=DESCRIPTIVE_REPRESENTATION_ITEM('Steel','Steel');
#3023=DESCRIPTIVE_REPRESENTATION_ITEM('Steel','Steel');
#3024=DESCRIPTIVE_REPRESENTATION_ITEM('Steel','Steel');
#3025=PROPERTY_DEFINITION('material property','material name',#13634);
#3026=PROPERTY_DEFINITION('material property','density of part',#13634);
#3027=PROPERTY_DEFINITION('material property','material name',#13635);
#3028=PROPERTY_DEFINITION('material property','density of part',#13635);
#3029=PROPERTY_DEFINITION('material property','material name',#13636);
#3030=PROPERTY_DEFINITION('material property','density of part',#13636);
#3031=PROPERTY_DEFINITION('material property','material name',#13637);
#3032=PROPERTY_DEFINITION('material property','density of part',#13637);
#3033=PROPERTY_DEFINITION('material property','material name',#13638);
#3034=PROPERTY_DEFINITION('material property','density of part',#13638);
#3035=PROPERTY_DEFINITION('material property','material name',#13639);
#3036=PROPERTY_DEFINITION('material property','density of part',#13639);
#3037=AXIS2_PLACEMENT_3D('',#3905,#3276,#3277);
#3038=AXIS2_PLACEMENT_3D('',#3906,#3278,#3279);
#3039=AXIS2_PLACEMENT_3D('',#3907,#3280,#3281);
#3040=AXIS2_PLACEMENT_3D('',#3908,#3282,#3283);
#3041=AXIS2_PLACEMENT_3D('',#3933,#3286,#3287);
#3042=AXIS2_PLACEMENT_3D('',#3971,#3289,#3290);
#3043=AXIS2_PLACEMENT_3D('',#4009,#3292,#3293);
#3044=AXIS2_PLACEMENT_3D('',#4047,#3295,#3296);
#3045=AXIS2_PLACEMENT_3D('',#4085,#3298,#3299);
#3046=AXIS2_PLACEMENT_3D('',#4123,#3301,#3302);
#3047=AXIS2_PLACEMENT_3D('',#4161,#3304,#3305);
#3048=AXIS2_PLACEMENT_3D('',#4199,#3307,#3308);
#3049=AXIS2_PLACEMENT_3D('',#4237,#3310,#3311);
#3050=AXIS2_PLACEMENT_3D('',#4275,#3313,#3314);
#3051=AXIS2_PLACEMENT_3D('',#4313,#3316,#3317);
#3052=AXIS2_PLACEMENT_3D('',#4351,#3319,#3320);
#3053=AXIS2_PLACEMENT_3D('',#4389,#3322,#3323);
#3054=AXIS2_PLACEMENT_3D('',#4427,#3325,#3326);
#3055=AXIS2_PLACEMENT_3D('',#4465,#3328,#3329);
#3056=AXIS2_PLACEMENT_3D('',#4503,#3331,#3332);
#3057=AXIS2_PLACEMENT_3D('',#4541,#3334,#3335);
#3058=AXIS2_PLACEMENT_3D('',#4579,#3337,#3338);
#3059=AXIS2_PLACEMENT_3D('',#4617,#3340,#3341);
#3060=AXIS2_PLACEMENT_3D('',#4655,#3343,#3344);
#3061=AXIS2_PLACEMENT_3D('',#4693,#3346,#3347);
#3062=AXIS2_PLACEMENT_3D('',#4731,#3349,#3350);
#3063=AXIS2_PLACEMENT_3D('',#4769,#3352,#3353);
#3064=AXIS2_PLACEMENT_3D('',#4807,#3355,#3356);
#3065=AXIS2_PLACEMENT_3D('',#4845,#3358,#3359);
#3066=AXIS2_PLACEMENT_3D('',#4883,#3361,#3362);
#3067=AXIS2_PLACEMENT_3D('',#4921,#3364,#3365);
#3068=AXIS2_PLACEMENT_3D('',#4959,#3367,#3368);
#3069=AXIS2_PLACEMENT_3D('',#4997,#3370,#3371);
#3070=AXIS2_PLACEMENT_3D('',#5035,#3373,#3374);
#3071=AXIS2_PLACEMENT_3D('',#5073,#3376,#3377);
#3072=AXIS2_PLACEMENT_3D('',#5111,#3379,#3380);
#3073=AXIS2_PLACEMENT_3D('',#5149,#3382,#3383);
#3074=AXIS2_PLACEMENT_3D('',#5187,#3385,#3386);
#3075=AXIS2_PLACEMENT_3D('',#5225,#3388,#3389);
#3076=AXIS2_PLACEMENT_3D('',#5263,#3391,#3392);
#3077=AXIS2_PLACEMENT_3D('',#5301,#3394,#3395);
#3078=AXIS2_PLACEMENT_3D('',#5339,#3397,#3398);
#3079=AXIS2_PLACEMENT_3D('',#5377,#3400,#3401);
#3080=AXIS2_PLACEMENT_3D('',#5415,#3403,#3404);
#3081=AXIS2_PLACEMENT_3D('',#5453,#3406,#3407);
#3082=AXIS2_PLACEMENT_3D('',#5491,#3409,#3410);
#3083=AXIS2_PLACEMENT_3D('',#5529,#3412,#3413);
#3084=AXIS2_PLACEMENT_3D('',#5567,#3415,#3416);
#3085=AXIS2_PLACEMENT_3D('',#5605,#3418,#3419);
#3086=AXIS2_PLACEMENT_3D('',#5643,#3421,#3422);
#3087=AXIS2_PLACEMENT_3D('',#5681,#3424,#3425);
#3088=AXIS2_PLACEMENT_3D('',#5719,#3427,#3428);
#3089=AXIS2_PLACEMENT_3D('',#5757,#3430,#3431);
#3090=AXIS2_PLACEMENT_3D('',#5782,#3434,#3435);
#3091=AXIS2_PLACEMENT_3D('',#5793,#3437,#3438);
#3092=AXIS2_PLACEMENT_3D('',#5801,#3439,#3440);
#3093=AXIS2_PLACEMENT_3D('',#5839,#3442,#3443);
#3094=AXIS2_PLACEMENT_3D('',#5877,#3445,#3446);
#3095=AXIS2_PLACEMENT_3D('',#5915,#3448,#3449);
#3096=AXIS2_PLACEMENT_3D('',#5953,#3451,#3452);
#3097=AXIS2_PLACEMENT_3D('',#5991,#3454,#3455);
#3098=AXIS2_PLACEMENT_3D('',#6029,#3457,#3458);
#3099=AXIS2_PLACEMENT_3D('',#6067,#3460,#3461);
#3100=AXIS2_PLACEMENT_3D('',#6105,#3463,#3464);
#3101=AXIS2_PLACEMENT_3D('',#6143,#3466,#3467);
#3102=AXIS2_PLACEMENT_3D('',#6181,#3469,#3470);
#3103=AXIS2_PLACEMENT_3D('',#6219,#3472,#3473);
#3104=AXIS2_PLACEMENT_3D('',#6257,#3475,#3476);
#3105=AXIS2_PLACEMENT_3D('',#6295,#3478,#3479);
#3106=AXIS2_PLACEMENT_3D('',#6333,#3481,#3482);
#3107=AXIS2_PLACEMENT_3D('',#6371,#3484,#3485);
#3108=AXIS2_PLACEMENT_3D('',#6409,#3487,#3488);
#3109=AXIS2_PLACEMENT_3D('',#6447,#3490,#3491);
#3110=AXIS2_PLACEMENT_3D('',#6485,#3493,#3494);
#3111=AXIS2_PLACEMENT_3D('',#6523,#3496,#3497);
#3112=AXIS2_PLACEMENT_3D('',#6561,#3499,#3500);
#3113=AXIS2_PLACEMENT_3D('',#6599,#3502,#3503);
#3114=AXIS2_PLACEMENT_3D('',#6637,#3505,#3506);
#3115=AXIS2_PLACEMENT_3D('',#6675,#3508,#3509);
#3116=AXIS2_PLACEMENT_3D('',#6713,#3511,#3512);
#3117=AXIS2_PLACEMENT_3D('',#6751,#3514,#3515);
#3118=AXIS2_PLACEMENT_3D('',#6789,#3517,#3518);
#3119=AXIS2_PLACEMENT_3D('',#6827,#3520,#3521);
#3120=AXIS2_PLACEMENT_3D('',#6865,#3523,#3524);
#3121=AXIS2_PLACEMENT_3D('',#6903,#3526,#3527);
#3122=AXIS2_PLACEMENT_3D('',#6941,#3529,#3530);
#3123=AXIS2_PLACEMENT_3D('',#6979,#3532,#3533);
#3124=AXIS2_PLACEMENT_3D('',#7017,#3535,#3536);
#3125=AXIS2_PLACEMENT_3D('',#7055,#3538,#3539);
#3126=AXIS2_PLACEMENT_3D('',#7093,#3541,#3542);
#3127=AXIS2_PLACEMENT_3D('',#7131,#3544,#3545);
#3128=AXIS2_PLACEMENT_3D('',#7169,#3547,#3548);
#3129=AXIS2_PLACEMENT_3D('',#7207,#3550,#3551);
#3130=AXIS2_PLACEMENT_3D('',#7245,#3553,#3554);
#3131=AXIS2_PLACEMENT_3D('',#7283,#3556,#3557);
#3132=AXIS2_PLACEMENT_3D('',#7321,#3559,#3560);
#3133=AXIS2_PLACEMENT_3D('',#7359,#3562,#3563);
#3134=AXIS2_PLACEMENT_3D('',#7397,#3565,#3566);
#3135=AXIS2_PLACEMENT_3D('',#7435,#3568,#3569);
#3136=AXIS2_PLACEMENT_3D('',#7473,#3571,#3572);
#3137=AXIS2_PLACEMENT_3D('',#7511,#3574,#3575);
#3138=AXIS2_PLACEMENT_3D('',#7549,#3577,#3578);
#3139=AXIS2_PLACEMENT_3D('',#7587,#3580,#3581);
#3140=AXIS2_PLACEMENT_3D('',#7589,#3582,#3583);
#3141=AXIS2_PLACEMENT_3D('',#7641,#3587,#3588);
#3142=AXIS2_PLACEMENT_3D('',#7644,#3589,#3590);
#3143=AXIS2_PLACEMENT_3D('',#7645,#3591,#3592);
#3144=AXIS2_PLACEMENT_3D('',#7648,#3594,#3595);
#3145=AXIS2_PLACEMENT_3D('',#7725,#3596,#3597);
#3146=AXIS2_PLACEMENT_3D('',#7760,#3598,#3599);
#3147=AXIS2_PLACEMENT_3D('',#7762,#3600,#3601);
#3148=AXIS2_PLACEMENT_3D('',#7764,#3602,#3603);
#3149=AXIS2_PLACEMENT_3D('',#7765,#3604,#3605);
#3150=AXIS2_PLACEMENT_3D('',#7767,#3606,#3607);
#3151=AXIS2_PLACEMENT_3D('',#7768,#3608,#3609);
#3152=AXIS2_PLACEMENT_3D('',#7769,#3610,#3611);
#3153=AXIS2_PLACEMENT_3D('',#7771,#3612,#3613);
#3154=AXIS2_PLACEMENT_3D('',#7772,#3614,#3615);
#3155=AXIS2_PLACEMENT_3D('',#7774,#3617,#3618);
#3156=AXIS2_PLACEMENT_3D('',#7777,#3621,#3622);
#3157=AXIS2_PLACEMENT_3D('',#9401,#3626,#3627);
#3158=AXIS2_PLACEMENT_3D('',#11036,#3628,#3629);
#3159=AXIS2_PLACEMENT_3D('',#11037,#3630,#3631);
#3160=AXIS2_PLACEMENT_3D('',#11040,#3633,#3634);
#3161=AXIS2_PLACEMENT_3D('',#11041,#3635,#3636);
#3162=AXIS2_PLACEMENT_3D('',#11042,#3637,#3638);
#3163=AXIS2_PLACEMENT_3D('',#11045,#3640,#3641);
#3164=AXIS2_PLACEMENT_3D('',#11046,#3642,#3643);
#3165=AXIS2_PLACEMENT_3D('',#11047,#3644,#3645);
#3166=AXIS2_PLACEMENT_3D('',#11049,#3647,#3648);
#3167=AXIS2_PLACEMENT_3D('',#11051,#3650,#3651);
#3168=AXIS2_PLACEMENT_3D('',#11052,#3652,#3653);
#3169=AXIS2_PLACEMENT_3D('',#11054,#3654,#3655);
#3170=AXIS2_PLACEMENT_3D('',#11055,#3656,#3657);
#3171=AXIS2_PLACEMENT_3D('',#11057,#3658,#3659);
#3172=AXIS2_PLACEMENT_3D('',#11060,#3661,#3662);
#3173=AXIS2_PLACEMENT_3D('',#11061,#3663,#3664);
#3174=AXIS2_PLACEMENT_3D('',#11063,#3665,#3666);
#3175=AXIS2_PLACEMENT_3D('',#11064,#3667,#3668);
#3176=AXIS2_PLACEMENT_3D('',#11066,#3669,#3670);
#3177=AXIS2_PLACEMENT_3D('',#11068,#3672,#3673);
#3178=AXIS2_PLACEMENT_3D('',#11069,#3674,#3675);
#3179=AXIS2_PLACEMENT_3D('',#11071,#3677,#3678);
#3180=AXIS2_PLACEMENT_3D('',#11072,#3679,#3680);
#3181=AXIS2_PLACEMENT_3D('',#11073,#3681,#3682);
#3182=AXIS2_PLACEMENT_3D('',#11074,#3683,#3684);
#3183=AXIS2_PLACEMENT_3D('',#11075,#3685,#3686);
#3184=AXIS2_PLACEMENT_3D('',#11140,#3688,#3689);
#3185=AXIS2_PLACEMENT_3D('',#11141,#3690,#3691);
#3186=AXIS2_PLACEMENT_3D('',#11143,#3692,#3693);
#3187=AXIS2_PLACEMENT_3D('',#11145,#3694,#3695);
#3188=AXIS2_PLACEMENT_3D('',#11146,#3696,#3697);
#3189=AXIS2_PLACEMENT_3D('',#11148,#3698,#3699);
#3190=AXIS2_PLACEMENT_3D('',#11150,#3700,#3701);
#3191=AXIS2_PLACEMENT_3D('',#11151,#3702,#3703);
#3192=AXIS2_PLACEMENT_3D('',#11215,#3705,#3706);
#3193=AXIS2_PLACEMENT_3D('',#11217,#3708,#3709);
#3194=AXIS2_PLACEMENT_3D('',#11219,#3710,#3711);
#3195=AXIS2_PLACEMENT_3D('',#11221,#3713,#3714);
#3196=AXIS2_PLACEMENT_3D('',#11223,#3715,#3716);
#3197=AXIS2_PLACEMENT_3D('',#11224,#3717,#3718);
#3198=AXIS2_PLACEMENT_3D('',#11226,#3719,#3720);
#3199=AXIS2_PLACEMENT_3D('',#11228,#3722,#3723);
#3200=AXIS2_PLACEMENT_3D('',#11230,#3724,#3725);
#3201=AXIS2_PLACEMENT_3D('',#11231,#3726,#3727);
#3202=AXIS2_PLACEMENT_3D('',#11234,#3729,#3730);
#3203=AXIS2_PLACEMENT_3D('',#11235,#3731,#3732);
#3204=AXIS2_PLACEMENT_3D('',#11236,#3733,#3734);
#3205=AXIS2_PLACEMENT_3D('',#11237,#3735,#3736);
#3206=AXIS2_PLACEMENT_3D('',#11239,#3737,#3738);
#3207=AXIS2_PLACEMENT_3D('',#11241,#3739,#3740);
#3208=AXIS2_PLACEMENT_3D('',#11242,#3741,#3742);
#3209=AXIS2_PLACEMENT_3D('',#11245,#3744,#3745);
#3210=AXIS2_PLACEMENT_3D('',#11246,#3746,#3747);
#3211=AXIS2_PLACEMENT_3D('',#11248,#3748,#3749);
#3212=AXIS2_PLACEMENT_3D('',#11250,#3751,#3752);
#3213=AXIS2_PLACEMENT_3D('',#11252,#3753,#3754);
#3214=AXIS2_PLACEMENT_3D('',#11254,#3756,#3757);
#3215=AXIS2_PLACEMENT_3D('',#11256,#3758,#3759);
#3216=AXIS2_PLACEMENT_3D('',#11259,#3761,#3762);
#3217=AXIS2_PLACEMENT_3D('',#11260,#3763,#3764);
#3218=AXIS2_PLACEMENT_3D('',#11261,#3765,#3766);
#3219=AXIS2_PLACEMENT_3D('',#11263,#3767,#3768);
#3220=AXIS2_PLACEMENT_3D('',#11266,#3770,#3771);
#3221=AXIS2_PLACEMENT_3D('',#11267,#3772,#3773);
#3222=AXIS2_PLACEMENT_3D('',#11268,#3774,#3775);
#3223=AXIS2_PLACEMENT_3D('',#11269,#3776,#3777);
#3224=AXIS2_PLACEMENT_3D('',#11270,#3778,#3779);
#3225=AXIS2_PLACEMENT_3D('',#11272,#3780,#3781);
#3226=AXIS2_PLACEMENT_3D('',#11274,#3782,#3783);
#3227=AXIS2_PLACEMENT_3D('',#11275,#3784,#3785);
#3228=AXIS2_PLACEMENT_3D('',#11278,#3786,#3787);
#3229=AXIS2_PLACEMENT_3D('',#11279,#3788,#3789);
#3230=AXIS2_PLACEMENT_3D('',#11280,#3790,#3791);
#3231=AXIS2_PLACEMENT_3D('',#11281,#3792,#3793);
#3232=AXIS2_PLACEMENT_3D('',#11283,#3794,#3795);
#3233=AXIS2_PLACEMENT_3D('',#11285,#3797,#3798);
#3234=AXIS2_PLACEMENT_3D('',#11287,#3799,#3800);
#3235=AXIS2_PLACEMENT_3D('',#11289,#3801,#3802);
#3236=AXIS2_PLACEMENT_3D('',#11290,#3803,#3804);
#3237=AXIS2_PLACEMENT_3D('',#11291,#3805,#3806);
#3238=AXIS2_PLACEMENT_3D('',#11294,#3808,#3809);
#3239=AXIS2_PLACEMENT_3D('',#11295,#3810,#3811);
#3240=AXIS2_PLACEMENT_3D('',#11297,#3812,#3813);
#3241=AXIS2_PLACEMENT_3D('',#11298,#3814,#3815);
#3242=AXIS2_PLACEMENT_3D('',#11300,#3816,#3817);
#3243=AXIS2_PLACEMENT_3D('',#11303,#3819,#3820);
#3244=AXIS2_PLACEMENT_3D('',#11304,#3821,#3822);
#3245=AXIS2_PLACEMENT_3D('',#11306,#3823,#3824);
#3246=AXIS2_PLACEMENT_3D('',#11309,#3826,#3827);
#3247=AXIS2_PLACEMENT_3D('',#11310,#3828,#3829);
#3248=AXIS2_PLACEMENT_3D('',#11311,#3830,#3831);
#3249=AXIS2_PLACEMENT_3D('',#11313,#3832,#3833);
#3250=AXIS2_PLACEMENT_3D('',#11314,#3834,#3835);
#3251=AXIS2_PLACEMENT_3D('',#11316,#3837,#3838);
#3252=AXIS2_PLACEMENT_3D('',#11317,#3839,#3840);
#3253=AXIS2_PLACEMENT_3D('',#11318,#3841,#3842);
#3254=AXIS2_PLACEMENT_3D('',#11368,#3845,#3846);
#3255=AXIS2_PLACEMENT_3D('',#11374,#3847,#3848);
#3256=AXIS2_PLACEMENT_3D('',#11379,#3849,#3850);
#3257=AXIS2_PLACEMENT_3D('',#11381,#3851,#3852);
#3258=AXIS2_PLACEMENT_3D('',#11744,#3854,#3855);
#3259=AXIS2_PLACEMENT_3D('',#12150,#3857,#3858);
#3260=AXIS2_PLACEMENT_3D('',#12555,#3859,#3860);
#3261=AXIS2_PLACEMENT_3D('',#12556,#3861,#3862);
#3262=AXIS2_PLACEMENT_3D('',#12567,#3865,#3866);
#3263=AXIS2_PLACEMENT_3D('',#13546,#3869,#3870);
#3264=AXIS2_PLACEMENT_3D('',#13549,#3871,#3872);
#3265=AXIS2_PLACEMENT_3D('',#13553,#3874,#3875);
#3266=AXIS2_PLACEMENT_3D('',#13555,#3877,#3878);
#3267=AXIS2_PLACEMENT_3D('',#13561,#3882,#3883);
#3268=AXIS2_PLACEMENT_3D('',#13567,#3887,#3888);
#3269=AXIS2_PLACEMENT_3D('',#13570,#3891,#3892);
#3270=AXIS2_PLACEMENT_3D('',#13571,#3893,#3894);
#3271=AXIS2_PLACEMENT_3D('',#13572,#3895,#3896);
#3272=AXIS2_PLACEMENT_3D('',#13573,#3897,#3898);
#3273=AXIS2_PLACEMENT_3D('',#13574,#3899,#3900);
#3274=AXIS2_PLACEMENT_3D('',#13575,#3901,#3902);
#3275=AXIS2_PLACEMENT_3D('',#13576,#3903,#3904);
#3276=DIRECTION('axis',(0.,0.,1.));
#3277=DIRECTION('refdir',(1.,0.,0.));
#3278=DIRECTION('axis',(0.,0.,1.));
#3279=DIRECTION('refdir',(1.,0.,0.));
#3280=DIRECTION('axis',(0.,0.,1.));
#3281=DIRECTION('refdir',(1.,0.,0.));
#3282=DIRECTION('center_axis',(0.,-1.,0.));
#3283=DIRECTION('ref_axis',(-1.,0.,5.80458639773891E-16));
#3284=DIRECTION('',(0.,-1.,0.));
#3285=DIRECTION('',(0.,-1.,0.));
#3286=DIRECTION('center_axis',(0.,-1.,0.));
#3287=DIRECTION('ref_axis',(-1.,0.,5.80458639773891E-16));
#3288=DIRECTION('',(0.,-1.,0.));
#3289=DIRECTION('center_axis',(0.,-1.,0.));
#3290=DIRECTION('ref_axis',(-1.,0.,5.80458639773891E-16));
#3291=DIRECTION('',(0.,-1.,0.));
#3292=DIRECTION('center_axis',(0.,-1.,0.));
#3293=DIRECTION('ref_axis',(-1.,0.,5.80458639773891E-16));
#3294=DIRECTION('',(0.,-1.,0.));
#3295=DIRECTION('center_axis',(0.,-1.,0.));
#3296=DIRECTION('ref_axis',(-1.,0.,5.80458639773891E-16));
#3297=DIRECTION('',(0.,-1.,0.));
#3298=DIRECTION('center_axis',(0.,-1.,0.));
#3299=DIRECTION('ref_axis',(-1.,0.,5.80458639773891E-16));
#3300=DIRECTION('',(0.,-1.,0.));
#3301=DIRECTION('center_axis',(0.,-1.,0.));
#3302=DIRECTION('ref_axis',(-1.,0.,5.80458639773891E-16));
#3303=DIRECTION('',(0.,-1.,0.));
#3304=DIRECTION('center_axis',(0.,-1.,0.));
#3305=DIRECTION('ref_axis',(-1.,0.,5.80458639773891E-16));
#3306=DIRECTION('',(0.,-1.,0.));
#3307=DIRECTION('center_axis',(0.,-1.,0.));
#3308=DIRECTION('ref_axis',(-1.,0.,5.80458639773891E-16));
#3309=DIRECTION('',(0.,-1.,0.));
#3310=DIRECTION('center_axis',(0.,-1.,0.));
#3311=DIRECTION('ref_axis',(-1.,0.,5.80458639773891E-16));
#3312=DIRECTION('',(0.,-1.,0.));
#3313=DIRECTION('center_axis',(0.,-1.,0.));
#3314=DIRECTION('ref_axis',(-1.,0.,5.80458639773891E-16));
#3315=DIRECTION('',(0.,-1.,0.));
#3316=DIRECTION('center_axis',(0.,-1.,0.));
#3317=DIRECTION('ref_axis',(-1.,0.,5.80458639773891E-16));
#3318=DIRECTION('',(0.,-1.,0.));
#3319=DIRECTION('center_axis',(0.,-1.,0.));
#3320=DIRECTION('ref_axis',(-1.,0.,5.80458639773891E-16));
#3321=DIRECTION('',(0.,-1.,0.));
#3322=DIRECTION('center_axis',(0.,-1.,0.));
#3323=DIRECTION('ref_axis',(-1.,0.,5.80458639773891E-16));
#3324=DIRECTION('',(0.,-1.,0.));
#3325=DIRECTION('center_axis',(0.,-1.,0.));
#3326=DIRECTION('ref_axis',(-1.,0.,5.80458639773891E-16));
#3327=DIRECTION('',(0.,-1.,0.));
#3328=DIRECTION('center_axis',(0.,-1.,0.));
#3329=DIRECTION('ref_axis',(-1.,0.,5.80458639773891E-16));
#3330=DIRECTION('',(0.,-1.,0.));
#3331=DIRECTION('center_axis',(0.,-1.,0.));
#3332=DIRECTION('ref_axis',(-1.,0.,5.80458639773891E-16));
#3333=DIRECTION('',(0.,-1.,0.));
#3334=DIRECTION('center_axis',(0.,-1.,0.));
#3335=DIRECTION('ref_axis',(-1.,0.,5.80458639773891E-16));
#3336=DIRECTION('',(0.,-1.,0.));
#3337=DIRECTION('center_axis',(0.,-1.,0.));
#3338=DIRECTION('ref_axis',(-1.,0.,5.80458639773891E-16));
#3339=DIRECTION('',(0.,-1.,0.));
#3340=DIRECTION('center_axis',(0.,-1.,0.));
#3341=DIRECTION('ref_axis',(-1.,0.,5.80458639773891E-16));
#3342=DIRECTION('',(0.,-1.,0.));
#3343=DIRECTION('center_axis',(0.,-1.,0.));
#3344=DIRECTION('ref_axis',(-1.,0.,5.80458639773891E-16));
#3345=DIRECTION('',(0.,-1.,0.));
#3346=DIRECTION('center_axis',(0.,-1.,0.));
#3347=DIRECTION('ref_axis',(-1.,0.,5.80458639773891E-16));
#3348=DIRECTION('',(0.,-1.,0.));
#3349=DIRECTION('center_axis',(0.,-1.,0.));
#3350=DIRECTION('ref_axis',(-1.,0.,5.80458639773891E-16));
#3351=DIRECTION('',(0.,-1.,0.));
#3352=DIRECTION('center_axis',(0.,-1.,0.));
#3353=DIRECTION('ref_axis',(-1.,0.,5.80458639773891E-16));
#3354=DIRECTION('',(0.,-1.,0.));
#3355=DIRECTION('center_axis',(0.,-1.,0.));
#3356=DIRECTION('ref_axis',(-1.,0.,5.80458639773891E-16));
#3357=DIRECTION('',(0.,-1.,0.));
#3358=DIRECTION('center_axis',(0.,-1.,0.));
#3359=DIRECTION('ref_axis',(-1.,0.,5.80458639773891E-16));
#3360=DIRECTION('',(0.,-1.,0.));
#3361=DIRECTION('center_axis',(0.,-1.,0.));
#3362=DIRECTION('ref_axis',(-1.,0.,5.80458639773891E-16));
#3363=DIRECTION('',(0.,-1.,0.));
#3364=DIRECTION('center_axis',(0.,-1.,0.));
#3365=DIRECTION('ref_axis',(-1.,0.,5.80458639773891E-16));
#3366=DIRECTION('',(0.,-1.,0.));
#3367=DIRECTION('center_axis',(0.,-1.,0.));
#3368=DIRECTION('ref_axis',(-1.,0.,5.80458639773891E-16));
#3369=DIRECTION('',(0.,-1.,0.));
#3370=DIRECTION('center_axis',(0.,-1.,0.));
#3371=DIRECTION('ref_axis',(-1.,0.,5.80458639773891E-16));
#3372=DIRECTION('',(0.,-1.,0.));
#3373=DIRECTION('center_axis',(0.,-1.,0.));
#3374=DIRECTION('ref_axis',(-1.,0.,5.80458639773891E-16));
#3375=DIRECTION('',(0.,-1.,0.));
#3376=DIRECTION('center_axis',(0.,-1.,0.));
#3377=DIRECTION('ref_axis',(-1.,0.,5.80458639773891E-16));
#3378=DIRECTION('',(0.,-1.,0.));
#3379=DIRECTION('center_axis',(0.,-1.,0.));
#3380=DIRECTION('ref_axis',(-1.,0.,5.80458639773891E-16));
#3381=DIRECTION('',(0.,-1.,0.));
#3382=DIRECTION('center_axis',(0.,-1.,0.));
#3383=DIRECTION('ref_axis',(-1.,0.,5.80458639773891E-16));
#3384=DIRECTION('',(0.,-1.,0.));
#3385=DIRECTION('center_axis',(0.,-1.,0.));
#3386=DIRECTION('ref_axis',(-1.,0.,5.80458639773891E-16));
#3387=DIRECTION('',(0.,-1.,0.));
#3388=DIRECTION('center_axis',(0.,-1.,0.));
#3389=DIRECTION('ref_axis',(-1.,0.,5.80458639773891E-16));
#3390=DIRECTION('',(0.,-1.,0.));
#3391=DIRECTION('center_axis',(0.,-1.,0.));
#3392=DIRECTION('ref_axis',(-1.,0.,5.80458639773891E-16));
#3393=DIRECTION('',(0.,-1.,0.));
#3394=DIRECTION('center_axis',(0.,-1.,0.));
#3395=DIRECTION('ref_axis',(-1.,0.,5.80458639773891E-16));
#3396=DIRECTION('',(0.,-1.,0.));
#3397=DIRECTION('center_axis',(0.,-1.,0.));
#3398=DIRECTION('ref_axis',(-1.,0.,5.80458639773891E-16));
#3399=DIRECTION('',(0.,-1.,0.));
#3400=DIRECTION('center_axis',(0.,-1.,0.));
#3401=DIRECTION('ref_axis',(-1.,0.,5.80458639773891E-16));
#3402=DIRECTION('',(0.,-1.,0.));
#3403=DIRECTION('center_axis',(0.,-1.,0.));
#3404=DIRECTION('ref_axis',(-1.,0.,5.80458639773891E-16));
#3405=DIRECTION('',(0.,-1.,0.));
#3406=DIRECTION('center_axis',(0.,-1.,0.));
#3407=DIRECTION('ref_axis',(-1.,0.,5.80458639773891E-16));
#3408=DIRECTION('',(0.,-1.,0.));
#3409=DIRECTION('center_axis',(0.,-1.,0.));
#3410=DIRECTION('ref_axis',(-1.,0.,5.80458639773891E-16));
#3411=DIRECTION('',(0.,-1.,0.));
#3412=DIRECTION('center_axis',(0.,-1.,0.));
#3413=DIRECTION('ref_axis',(-1.,0.,5.80458639773891E-16));
#3414=DIRECTION('',(0.,-1.,0.));
#3415=DIRECTION('center_axis',(0.,-1.,0.));
#3416=DIRECTION('ref_axis',(-1.,0.,5.80458639773891E-16));
#3417=DIRECTION('',(0.,-1.,0.));
#3418=DIRECTION('center_axis',(0.,-1.,0.));
#3419=DIRECTION('ref_axis',(-1.,0.,5.80458639773891E-16));
#3420=DIRECTION('',(0.,-1.,0.));
#3421=DIRECTION('center_axis',(0.,-1.,0.));
#3422=DIRECTION('ref_axis',(-1.,0.,5.80458639773891E-16));
#3423=DIRECTION('',(0.,-1.,0.));
#3424=DIRECTION('center_axis',(0.,-1.,0.));
#3425=DIRECTION('ref_axis',(-1.,0.,5.80458639773891E-16));
#3426=DIRECTION('',(0.,-1.,0.));
#3427=DIRECTION('center_axis',(0.,-1.,0.));
#3428=DIRECTION('ref_axis',(-1.,0.,5.80458639773891E-16));
#3429=DIRECTION('',(0.,-1.,0.));
#3430=DIRECTION('center_axis',(0.,-1.,0.));
#3431=DIRECTION('ref_axis',(-1.,0.,5.80458639773891E-16));
#3432=DIRECTION('',(0.,-1.,0.));
#3433=DIRECTION('',(0.,1.,0.));
#3434=DIRECTION('center_axis',(0.,-1.,0.));
#3435=DIRECTION('ref_axis',(0.,0.,-1.));
#3436=DIRECTION('',(0.,-1.,0.));
#3437=DIRECTION('center_axis',(0.,1.,0.));
#3438=DIRECTION('ref_axis',(0.,0.,1.));
#3439=DIRECTION('center_axis',(0.,-1.,0.));
#3440=DIRECTION('ref_axis',(0.,0.,-1.));
#3441=DIRECTION('',(0.,-1.,0.));
#3442=DIRECTION('center_axis',(0.,-1.,0.));
#3443=DIRECTION('ref_axis',(0.,0.,-1.));
#3444=DIRECTION('',(0.,-1.,0.));
#3445=DIRECTION('center_axis',(0.,-1.,0.));
#3446=DIRECTION('ref_axis',(0.,0.,-1.));
#3447=DIRECTION('',(0.,-1.,0.));
#3448=DIRECTION('center_axis',(0.,-1.,0.));
#3449=DIRECTION('ref_axis',(0.,0.,-1.));
#3450=DIRECTION('',(0.,-1.,0.));
#3451=DIRECTION('center_axis',(0.,-1.,0.));
#3452=DIRECTION('ref_axis',(0.,0.,-1.));
#3453=DIRECTION('',(0.,-1.,0.));
#3454=DIRECTION('center_axis',(0.,-1.,0.));
#3455=DIRECTION('ref_axis',(0.,0.,-1.));
#3456=DIRECTION('',(0.,-1.,0.));
#3457=DIRECTION('center_axis',(0.,-1.,0.));
#3458=DIRECTION('ref_axis',(0.,0.,-1.));
#3459=DIRECTION('',(0.,-1.,0.));
#3460=DIRECTION('center_axis',(0.,-1.,0.));
#3461=DIRECTION('ref_axis',(0.,0.,-1.));
#3462=DIRECTION('',(0.,-1.,0.));
#3463=DIRECTION('center_axis',(0.,-1.,0.));
#3464=DIRECTION('ref_axis',(0.,0.,-1.));
#3465=DIRECTION('',(0.,-1.,0.));
#3466=DIRECTION('center_axis',(0.,-1.,0.));
#3467=DIRECTION('ref_axis',(0.,0.,-1.));
#3468=DIRECTION('',(0.,-1.,0.));
#3469=DIRECTION('center_axis',(0.,-1.,0.));
#3470=DIRECTION('ref_axis',(0.,0.,-1.));
#3471=DIRECTION('',(0.,-1.,0.));
#3472=DIRECTION('center_axis',(0.,-1.,0.));
#3473=DIRECTION('ref_axis',(0.,0.,-1.));
#3474=DIRECTION('',(0.,-1.,0.));
#3475=DIRECTION('center_axis',(0.,-1.,0.));
#3476=DIRECTION('ref_axis',(0.,0.,-1.));
#3477=DIRECTION('',(0.,-1.,0.));
#3478=DIRECTION('center_axis',(0.,-1.,0.));
#3479=DIRECTION('ref_axis',(0.,0.,-1.));
#3480=DIRECTION('',(0.,-1.,0.));
#3481=DIRECTION('center_axis',(0.,-1.,0.));
#3482=DIRECTION('ref_axis',(0.,0.,-1.));
#3483=DIRECTION('',(0.,-1.,0.));
#3484=DIRECTION('center_axis',(0.,-1.,0.));
#3485=DIRECTION('ref_axis',(0.,0.,-1.));
#3486=DIRECTION('',(0.,-1.,0.));
#3487=DIRECTION('center_axis',(0.,-1.,0.));
#3488=DIRECTION('ref_axis',(0.,0.,-1.));
#3489=DIRECTION('',(0.,-1.,0.));
#3490=DIRECTION('center_axis',(0.,-1.,0.));
#3491=DIRECTION('ref_axis',(0.,0.,-1.));
#3492=DIRECTION('',(0.,-1.,0.));
#3493=DIRECTION('center_axis',(0.,-1.,0.));
#3494=DIRECTION('ref_axis',(0.,0.,-1.));
#3495=DIRECTION('',(0.,-1.,0.));
#3496=DIRECTION('center_axis',(0.,-1.,0.));
#3497=DIRECTION('ref_axis',(0.,0.,-1.));
#3498=DIRECTION('',(0.,-1.,0.));
#3499=DIRECTION('center_axis',(0.,-1.,0.));
#3500=DIRECTION('ref_axis',(0.,0.,-1.));
#3501=DIRECTION('',(0.,-1.,0.));
#3502=DIRECTION('center_axis',(0.,-1.,0.));
#3503=DIRECTION('ref_axis',(0.,0.,-1.));
#3504=DIRECTION('',(0.,-1.,0.));
#3505=DIRECTION('center_axis',(0.,-1.,0.));
#3506=DIRECTION('ref_axis',(0.,0.,-1.));
#3507=DIRECTION('',(0.,-1.,0.));
#3508=DIRECTION('center_axis',(0.,-1.,0.));
#3509=DIRECTION('ref_axis',(0.,0.,-1.));
#3510=DIRECTION('',(0.,-1.,0.));
#3511=DIRECTION('center_axis',(0.,-1.,0.));
#3512=DIRECTION('ref_axis',(0.,0.,-1.));
#3513=DIRECTION('',(0.,-1.,0.));
#3514=DIRECTION('center_axis',(0.,-1.,0.));
#3515=DIRECTION('ref_axis',(0.,0.,-1.));
#3516=DIRECTION('',(0.,-1.,0.));
#3517=DIRECTION('center_axis',(0.,-1.,0.));
#3518=DIRECTION('ref_axis',(0.,0.,-1.));
#3519=DIRECTION('',(0.,-1.,0.));
#3520=DIRECTION('center_axis',(0.,-1.,0.));
#3521=DIRECTION('ref_axis',(0.,0.,-1.));
#3522=DIRECTION('',(0.,-1.,0.));
#3523=DIRECTION('center_axis',(0.,-1.,0.));
#3524=DIRECTION('ref_axis',(0.,0.,-1.));
#3525=DIRECTION('',(0.,-1.,0.));
#3526=DIRECTION('center_axis',(0.,-1.,0.));
#3527=DIRECTION('ref_axis',(0.,0.,-1.));
#3528=DIRECTION('',(0.,-1.,0.));
#3529=DIRECTION('center_axis',(0.,-1.,0.));
#3530=DIRECTION('ref_axis',(0.,0.,-1.));
#3531=DIRECTION('',(0.,-1.,0.));
#3532=DIRECTION('center_axis',(0.,-1.,0.));
#3533=DIRECTION('ref_axis',(0.,0.,-1.));
#3534=DIRECTION('',(0.,-1.,0.));
#3535=DIRECTION('center_axis',(0.,-1.,0.));
#3536=DIRECTION('ref_axis',(0.,0.,-1.));
#3537=DIRECTION('',(0.,-1.,0.));
#3538=DIRECTION('center_axis',(0.,-1.,0.));
#3539=DIRECTION('ref_axis',(0.,0.,-1.));
#3540=DIRECTION('',(0.,-1.,0.));
#3541=DIRECTION('center_axis',(0.,-1.,0.));
#3542=DIRECTION('ref_axis',(0.,0.,-1.));
#3543=DIRECTION('',(0.,-1.,0.));
#3544=DIRECTION('center_axis',(0.,-1.,0.));
#3545=DIRECTION('ref_axis',(0.,0.,-1.));
#3546=DIRECTION('',(0.,-1.,0.));
#3547=DIRECTION('center_axis',(0.,-1.,0.));
#3548=DIRECTION('ref_axis',(0.,0.,-1.));
#3549=DIRECTION('',(0.,-1.,0.));
#3550=DIRECTION('center_axis',(0.,-1.,0.));
#3551=DIRECTION('ref_axis',(0.,0.,-1.));
#3552=DIRECTION('',(0.,-1.,0.));
#3553=DIRECTION('center_axis',(0.,-1.,0.));
#3554=DIRECTION('ref_axis',(0.,0.,-1.));
#3555=DIRECTION('',(0.,-1.,0.));
#3556=DIRECTION('center_axis',(0.,-1.,0.));
#3557=DIRECTION('ref_axis',(0.,0.,-1.));
#3558=DIRECTION('',(0.,-1.,0.));
#3559=DIRECTION('center_axis',(0.,-1.,0.));
#3560=DIRECTION('ref_axis',(0.,0.,-1.));
#3561=DIRECTION('',(0.,-1.,0.));
#3562=DIRECTION('center_axis',(0.,-1.,0.));
#3563=DIRECTION('ref_axis',(0.,0.,-1.));
#3564=DIRECTION('',(0.,-1.,0.));
#3565=DIRECTION('center_axis',(0.,-1.,0.));
#3566=DIRECTION('ref_axis',(0.,0.,-1.));
#3567=DIRECTION('',(0.,-1.,0.));
#3568=DIRECTION('center_axis',(0.,-1.,0.));
#3569=DIRECTION('ref_axis',(0.,0.,-1.));
#3570=DIRECTION('',(0.,-1.,0.));
#3571=DIRECTION('center_axis',(0.,-1.,0.));
#3572=DIRECTION('ref_axis',(0.,0.,-1.));
#3573=DIRECTION('',(0.,-1.,0.));
#3574=DIRECTION('center_axis',(0.,-1.,0.));
#3575=DIRECTION('ref_axis',(0.,0.,-1.));
#3576=DIRECTION('',(0.,-1.,0.));
#3577=DIRECTION('center_axis',(0.,-1.,0.));
#3578=DIRECTION('ref_axis',(0.,0.,-1.));
#3579=DIRECTION('',(0.,-1.,0.));
#3580=DIRECTION('center_axis',(0.,-1.,0.));
#3581=DIRECTION('ref_axis',(0.,0.,-1.));
#3582=DIRECTION('center_axis',(0.,1.,0.));
#3583=DIRECTION('ref_axis',(0.,0.,1.));
#3584=DIRECTION('',(0.,-1.,0.));
#3585=DIRECTION('',(0.,-1.,0.));
#3586=DIRECTION('',(0.,-1.,0.));
#3587=DIRECTION('center_axis',(0.,-1.,0.));
#3588=DIRECTION('ref_axis',(0.,0.,-1.));
#3589=DIRECTION('center_axis',(0.,1.,0.));
#3590=DIRECTION('ref_axis',(0.,0.,1.));
#3591=DIRECTION('center_axis',(0.,1.,0.));
#3592=DIRECTION('ref_axis',(0.,0.,1.));
#3593=DIRECTION('',(0.,1.,0.));
#3594=DIRECTION('center_axis',(0.,1.,0.));
#3595=DIRECTION('ref_axis',(0.,0.,1.));
#3596=DIRECTION('center_axis',(0.,-1.,0.));
#3597=DIRECTION('ref_axis',(0.,0.,-1.));
#3598=DIRECTION('center_axis',(0.,1.,0.));
#3599=DIRECTION('ref_axis',(0.,0.,1.));
#3600=DIRECTION('center_axis',(0.,1.,0.));
#3601=DIRECTION('ref_axis',(0.,0.,1.));
#3602=DIRECTION('center_axis',(0.,1.,0.));
#3603=DIRECTION('ref_axis',(0.,0.,1.));
#3604=DIRECTION('center_axis',(0.,1.,0.));
#3605=DIRECTION('ref_axis',(0.,0.,1.));
#3606=DIRECTION('center_axis',(0.,1.,0.));
#3607=DIRECTION('ref_axis',(0.,0.,1.));
#3608=DIRECTION('center_axis',(0.,1.,0.));
#3609=DIRECTION('ref_axis',(0.,0.,1.));
#3610=DIRECTION('center_axis',(0.,1.,0.));
#3611=DIRECTION('ref_axis',(0.,0.,1.));
#3612=DIRECTION('center_axis',(0.,1.,0.));
#3613=DIRECTION('ref_axis',(0.,0.,1.));
#3614=DIRECTION('center_axis',(0.,-1.,0.));
#3615=DIRECTION('ref_axis',(0.,0.,-1.));
#3616=DIRECTION('',(5.17558101501968E-17,0.906307787036649,-0.422618261740701));
#3617=DIRECTION('center_axis',(0.,0.,1.));
#3618=DIRECTION('ref_axis',(1.,0.,0.));
#3619=DIRECTION('',(-0.866025403784442,0.499999999999994,0.));
#3620=DIRECTION('',(0.866025403784448,0.499999999999983,0.));
#3621=DIRECTION('center_axis',(0.,0.,-1.));
#3622=DIRECTION('ref_axis',(-1.,0.,0.));
#3623=DIRECTION('',(0.866025403784442,-0.499999999999995,0.));
#3624=DIRECTION('',(-0.866025403784444,-0.499999999999991,0.));
#3625=DIRECTION('',(0.,1.,0.));
#3626=DIRECTION('center_axis',(0.,-1.,0.));
#3627=DIRECTION('ref_axis',(-1.,0.,5.80458639773891E-16));
#3628=DIRECTION('center_axis',(0.,-1.,0.));
#3629=DIRECTION('ref_axis',(0.923879529047881,0.,0.382683440726491));
#3630=DIRECTION('center_axis',(-1.,0.,0.));
#3631=DIRECTION('ref_axis',(0.,0.,1.));
#3632=DIRECTION('',(-1.,0.,0.));
#3633=DIRECTION('center_axis',(-1.,0.,0.));
#3634=DIRECTION('ref_axis',(0.,0.,1.));
#3635=DIRECTION('center_axis',(1.,0.,0.));
#3636=DIRECTION('ref_axis',(0.,0.,-1.));
#3637=DIRECTION('center_axis',(1.,0.,0.));
#3638=DIRECTION('ref_axis',(0.,0.,1.));
#3639=DIRECTION('',(1.,0.,0.));
#3640=DIRECTION('center_axis',(-1.,0.,0.));
#3641=DIRECTION('ref_axis',(0.,0.,1.));
#3642=DIRECTION('center_axis',(-1.,0.,0.));
#3643=DIRECTION('ref_axis',(0.,0.,1.));
#3644=DIRECTION('center_axis',(0.,1.,0.));
#3645=DIRECTION('ref_axis',(0.,0.,1.));
#3646=DIRECTION('',(-1.70437892618156E-17,0.99026806874157,-0.139173100960066));
#3647=DIRECTION('center_axis',(0.,1.,0.));
#3648=DIRECTION('ref_axis',(0.,0.,1.));
#3649=DIRECTION('',(6.1232339957367E-17,-0.866025403784442,0.499999999999995));
#3650=DIRECTION('axis',(0.,0.,1.));
#3651=DIRECTION('refdir',(1.,0.,0.));
#3652=DIRECTION('center_axis',(-1.,0.,0.));
#3653=DIRECTION('ref_axis',(0.,0.,1.));
#3654=DIRECTION('center_axis',(-1.,0.,0.));
#3655=DIRECTION('ref_axis',(0.,0.,1.));
#3656=DIRECTION('center_axis',(-1.,0.,0.));
#3657=DIRECTION('ref_axis',(0.,0.,1.));
#3658=DIRECTION('center_axis',(-1.,0.,0.));
#3659=DIRECTION('ref_axis',(0.,0.,1.));
#3660=DIRECTION('',(1.,0.,0.));
#3661=DIRECTION('center_axis',(-1.,0.,0.));
#3662=DIRECTION('ref_axis',(0.,0.,1.));
#3663=DIRECTION('center_axis',(1.,0.,0.));
#3664=DIRECTION('ref_axis',(0.,0.,-1.));
#3665=DIRECTION('center_axis',(-1.,0.,0.));
#3666=DIRECTION('ref_axis',(0.,0.,1.));
#3667=DIRECTION('center_axis',(-1.,0.,0.));
#3668=DIRECTION('ref_axis',(0.,0.,1.));
#3669=DIRECTION('center_axis',(-1.,0.,0.));
#3670=DIRECTION('ref_axis',(0.,0.,1.));
#3671=DIRECTION('',(1.,0.,0.));
#3672=DIRECTION('center_axis',(1.,0.,0.));
#3673=DIRECTION('ref_axis',(0.,0.,-1.));
#3674=DIRECTION('center_axis',(-1.,0.,0.));
#3675=DIRECTION('ref_axis',(0.,0.,1.));
#3676=DIRECTION('',(0.707106781186545,8.65956056235497E-17,0.70710678118655));
#3677=DIRECTION('',(0.,0.,1.));
#3678=DIRECTION('',(1.,0.,0.));
#3679=DIRECTION('',(0.,-0.0346780139270669,0.999398536796044));
#3680=DIRECTION('',(1.,0.,0.));
#3681=DIRECTION('',(0.,-0.936910481643036,-0.3495693770733));
#3682=DIRECTION('',(-1.,0.,0.));
#3683=DIRECTION('axis',(0.,0.,1.));
#3684=DIRECTION('refdir',(1.,0.,0.));
#3685=DIRECTION('center_axis',(1.73472347597681E-16,1.,0.));
#3686=DIRECTION('ref_axis',(-1.,1.73472347597681E-16,0.));
#3687=DIRECTION('',(1.73472347597681E-16,1.,0.));
#3688=DIRECTION('center_axis',(1.73472347597681E-16,1.,0.));
#3689=DIRECTION('ref_axis',(-1.,1.73472347597681E-16,0.));
#3690=DIRECTION('center_axis',(0.,0.,-1.));
#3691=DIRECTION('ref_axis',(-1.,0.,0.));
#3692=DIRECTION('center_axis',(0.,0.,-1.));
#3693=DIRECTION('ref_axis',(-1.,0.,0.));
#3694=DIRECTION('center_axis',(0.,0.,-1.));
#3695=DIRECTION('ref_axis',(-1.,0.,0.));
#3696=DIRECTION('center_axis',(0.,0.,-1.));
#3697=DIRECTION('ref_axis',(-1.,0.,0.));
#3698=DIRECTION('center_axis',(0.,0.,-1.));
#3699=DIRECTION('ref_axis',(-1.,0.,0.));
#3700=DIRECTION('center_axis',(0.,0.,-1.));
#3701=DIRECTION('ref_axis',(-1.,0.,0.));
#3702=DIRECTION('center_axis',(0.,0.,-1.));
#3703=DIRECTION('ref_axis',(-1.,0.,0.));
#3704=DIRECTION('',(0.,0.,1.));
#3705=DIRECTION('center_axis',(0.,0.,-1.));
#3706=DIRECTION('ref_axis',(-1.,0.,0.));
#3707=DIRECTION('',(0.,0.,-1.));
#3708=DIRECTION('center_axis',(1.73472347597681E-16,1.,0.));
#3709=DIRECTION('ref_axis',(-1.,1.73472347597681E-16,0.));
#3710=DIRECTION('center_axis',(1.73472347597681E-16,1.,0.));
#3711=DIRECTION('ref_axis',(-1.,1.73472347597681E-16,0.));
#3712=DIRECTION('',(-1.73472347597681E-16,-1.,0.));
#3713=DIRECTION('center_axis',(1.73472347597681E-16,1.,0.));
#3714=DIRECTION('ref_axis',(0.,0.,1.));
#3715=DIRECTION('center_axis',(1.73472347597681E-16,1.,0.));
#3716=DIRECTION('ref_axis',(1.,-1.73472347597681E-16,0.));
#3717=DIRECTION('center_axis',(1.73472347597681E-16,1.,0.));
#3718=DIRECTION('ref_axis',(-1.,1.73472347597681E-16,0.));
#3719=DIRECTION('center_axis',(1.73472347597681E-16,1.,0.));
#3720=DIRECTION('ref_axis',(-1.,1.73472347597681E-16,0.));
#3721=DIRECTION('',(-1.73472347597681E-16,-1.,0.));
#3722=DIRECTION('center_axis',(1.73472347597681E-16,1.,0.));
#3723=DIRECTION('ref_axis',(0.,0.,1.));
#3724=DIRECTION('center_axis',(1.73472347597681E-16,1.,0.));
#3725=DIRECTION('ref_axis',(1.,-1.73472347597681E-16,0.));
#3726=DIRECTION('center_axis',(1.73472347597681E-16,1.,0.));
#3727=DIRECTION('ref_axis',(-1.,1.73472347597681E-16,0.));
#3728=DIRECTION('',(1.73472347597681E-16,1.,0.));
#3729=DIRECTION('center_axis',(1.73472347597681E-16,1.,0.));
#3730=DIRECTION('ref_axis',(1.,-1.73472347597681E-16,0.));
#3731=DIRECTION('center_axis',(1.73472347597681E-16,1.,0.));
#3732=DIRECTION('ref_axis',(0.,0.,1.));
#3733=DIRECTION('axis',(0.,0.,1.));
#3734=DIRECTION('refdir',(1.,0.,0.));
#3735=DIRECTION('center_axis',(0.,-1.,0.));
#3736=DIRECTION('ref_axis',(0.,0.,-1.));
#3737=DIRECTION('center_axis',(0.,1.,0.));
#3738=DIRECTION('ref_axis',(0.,0.,1.));
#3739=DIRECTION('center_axis',(0.,1.,0.));
#3740=DIRECTION('ref_axis',(0.,0.,1.));
#3741=DIRECTION('center_axis',(0.,1.,0.));
#3742=DIRECTION('ref_axis',(0.,0.,1.));
#3743=DIRECTION('',(5.47678698264202E-17,-0.894427190999916,0.447213595499958));
#3744=DIRECTION('center_axis',(0.,-1.,0.));
#3745=DIRECTION('ref_axis',(0.,0.,-1.));
#3746=DIRECTION('center_axis',(0.,1.,0.));
#3747=DIRECTION('ref_axis',(0.,0.,1.));
#3748=DIRECTION('center_axis',(0.,1.,0.));
#3749=DIRECTION('ref_axis',(0.,0.,1.));
#3750=DIRECTION('',(-5.47678698264202E-17,0.894427190999916,-0.447213595499958));
#3751=DIRECTION('center_axis',(0.,1.,0.));
#3752=DIRECTION('ref_axis',(0.,0.,1.));
#3753=DIRECTION('center_axis',(0.,-1.,0.));
#3754=DIRECTION('ref_axis',(0.,0.,-1.));
#3755=DIRECTION('',(0.,1.,0.));
#3756=DIRECTION('center_axis',(0.,1.,0.));
#3757=DIRECTION('ref_axis',(0.,0.,1.));
#3758=DIRECTION('center_axis',(0.,-1.,0.));
#3759=DIRECTION('ref_axis',(0.,0.,-1.));
#3760=DIRECTION('',(0.,-1.,0.));
#3761=DIRECTION('center_axis',(0.,-1.,0.));
#3762=DIRECTION('ref_axis',(0.,0.,-1.));
#3763=DIRECTION('center_axis',(0.,-1.,0.));
#3764=DIRECTION('ref_axis',(0.,0.,-1.));
#3765=DIRECTION('center_axis',(0.,1.,0.));
#3766=DIRECTION('ref_axis',(0.,0.,1.));
#3767=DIRECTION('center_axis',(0.,-1.,0.));
#3768=DIRECTION('ref_axis',(0.,0.,-1.));
#3769=DIRECTION('',(0.,-1.,0.));
#3770=DIRECTION('center_axis',(0.,-1.,0.));
#3771=DIRECTION('ref_axis',(0.,0.,-1.));
#3772=DIRECTION('center_axis',(0.,-1.,0.));
#3773=DIRECTION('ref_axis',(0.,0.,-1.));
#3774=DIRECTION('center_axis',(0.,-1.,0.));
#3775=DIRECTION('ref_axis',(0.,0.,-1.));
#3776=DIRECTION('axis',(0.,0.,1.));
#3777=DIRECTION('refdir',(1.,0.,0.));
#3778=DIRECTION('center_axis',(1.73472347597681E-16,-1.,-5.55111512312578E-16));
#3779=DIRECTION('ref_axis',(0.,5.55111512312578E-16,-1.));
#3780=DIRECTION('center_axis',(1.73472347597681E-16,-1.,-5.55111512312578E-16));
#3781=DIRECTION('ref_axis',(-1.,-1.73472347597681E-16,-9.62964972193618E-32));
#3782=DIRECTION('center_axis',(1.73472347597681E-16,-1.,-5.55111512312578E-16));
#3783=DIRECTION('ref_axis',(0.,5.55111512312578E-16,-1.));
#3784=DIRECTION('center_axis',(1.,0.,0.));
#3785=DIRECTION('ref_axis',(0.,0.,-1.));
#3786=DIRECTION('center_axis',(1.73472347597681E-16,1.,0.));
#3787=DIRECTION('ref_axis',(-1.,1.73472347597681E-16,0.));
#3788=DIRECTION('center_axis',(1.73472347597681E-16,1.,0.));
#3789=DIRECTION('ref_axis',(-1.,1.73472347597681E-16,0.));
#3790=DIRECTION('center_axis',(-1.,0.,0.));
#3791=DIRECTION('ref_axis',(0.,0.,-1.));
#3792=DIRECTION('center_axis',(0.,-1.,-1.38777878078145E-16));
#3793=DIRECTION('ref_axis',(0.,1.38777878078145E-16,-1.));
#3794=DIRECTION('center_axis',(1.73472347597681E-16,1.,0.));
#3795=DIRECTION('ref_axis',(-1.,1.73472347597681E-16,0.));
#3796=DIRECTION('',(0.,1.,1.38777878078145E-16));
#3797=DIRECTION('center_axis',(1.,0.,0.));
#3798=DIRECTION('ref_axis',(0.,0.,-1.));
#3799=DIRECTION('center_axis',(1.,0.,0.));
#3800=DIRECTION('ref_axis',(0.,0.,-1.));
#3801=DIRECTION('center_axis',(0.,1.,3.43024899888577E-15));
#3802=DIRECTION('ref_axis',(0.,-3.43024899888577E-15,1.));
#3803=DIRECTION('center_axis',(0.,1.,3.43024899888577E-15));
#3804=DIRECTION('ref_axis',(0.,-3.43024899888577E-15,1.));
#3805=DIRECTION('center_axis',(0.,-1.,-1.38777878078145E-16));
#3806=DIRECTION('ref_axis',(0.,1.38777878078145E-16,-1.));
#3807=DIRECTION('',(0.,-1.,-1.38777878078145E-16));
#3808=DIRECTION('center_axis',(1.73472347597681E-16,1.,0.));
#3809=DIRECTION('ref_axis',(-1.,1.73472347597681E-16,0.));
#3810=DIRECTION('center_axis',(1.73472347597681E-16,1.,0.));
#3811=DIRECTION('ref_axis',(0.,0.,1.));
#3812=DIRECTION('center_axis',(1.73472347597681E-16,1.,0.));
#3813=DIRECTION('ref_axis',(1.,-1.73472347597681E-16,0.));
#3814=DIRECTION('center_axis',(-1.73472347597681E-16,-1.,0.));
#3815=DIRECTION('ref_axis',(1.,-1.73472347597681E-16,0.));
#3816=DIRECTION('center_axis',(1.73472347597681E-16,1.,0.));
#3817=DIRECTION('ref_axis',(-1.,1.73472347597681E-16,0.));
#3818=DIRECTION('',(1.73472347597681E-16,1.,0.));
#3819=DIRECTION('center_axis',(1.73472347597681E-16,1.,0.));
#3820=DIRECTION('ref_axis',(-1.,1.73472347597681E-16,0.));
#3821=DIRECTION('center_axis',(-1.73472347597681E-16,-1.,0.));
#3822=DIRECTION('ref_axis',(1.,-1.73472347597681E-16,0.));
#3823=DIRECTION('center_axis',(1.73472347597681E-16,1.,0.));
#3824=DIRECTION('ref_axis',(-1.,1.73472347597681E-16,0.));
#3825=DIRECTION('',(-1.73472347597681E-16,-1.,0.));
#3826=DIRECTION('center_axis',(1.73472347597681E-16,1.,0.));
#3827=DIRECTION('ref_axis',(1.,-1.73472347597681E-16,0.));
#3828=DIRECTION('center_axis',(1.73472347597681E-16,1.,0.));
#3829=DIRECTION('ref_axis',(0.,0.,1.));
#3830=DIRECTION('center_axis',(1.73472347597681E-16,1.,0.));
#3831=DIRECTION('ref_axis',(0.,0.,1.));
#3832=DIRECTION('center_axis',(1.73472347597681E-16,1.,0.));
#3833=DIRECTION('ref_axis',(1.,-1.73472347597681E-16,0.));
#3834=DIRECTION('center_axis',(1.73472347597681E-16,1.,0.));
#3835=DIRECTION('ref_axis',(-1.,1.73472347597681E-16,0.));
#3836=DIRECTION('',(1.73472347597681E-16,1.,0.));
#3837=DIRECTION('center_axis',(1.73472347597681E-16,1.,0.));
#3838=DIRECTION('ref_axis',(0.,0.,1.));
#3839=DIRECTION('axis',(0.,0.,1.));
#3840=DIRECTION('refdir',(1.,0.,0.));
#3841=DIRECTION('center_axis',(0.,-1.,0.));
#3842=DIRECTION('ref_axis',(0.,0.,-1.));
#3843=DIRECTION('',(0.,1.,0.));
#3844=DIRECTION('',(0.,1.,0.));
#3845=DIRECTION('center_axis',(0.,1.,0.));
#3846=DIRECTION('ref_axis',(0.,0.,1.));
#3847=DIRECTION('center_axis',(0.997979715186782,0.0635333619109602,1.57664132857237E-12));
#3848=DIRECTION('ref_axis',(0.000102666233862281,-0.00161267745569481,0.999998694364682));
#3849=DIRECTION('center_axis',(0.,-1.,0.));
#3850=DIRECTION('ref_axis',(0.,0.,-1.));
#3851=DIRECTION('center_axis',(0.,1.,0.));
#3852=DIRECTION('ref_axis',(0.,0.,1.));
#3853=DIRECTION('',(0.,1.,0.));
#3854=DIRECTION('center_axis',(-0.997979715186782,-0.0635333619109597,-1.60052983355074E-12));
#3855=DIRECTION('ref_axis',(1.40886995536597E-7,-2.21307290245903E-6,0.999999999997541));
#3856=DIRECTION('',(0.,1.,0.));
#3857=DIRECTION('center_axis',(0.,-1.,0.));
#3858=DIRECTION('ref_axis',(0.,0.,-1.));
#3859=DIRECTION('center_axis',(0.,1.,0.));
#3860=DIRECTION('ref_axis',(0.,0.,1.));
#3861=DIRECTION('center_axis',(-0.997979715186782,-0.0635333619109615,0.));
#3862=DIRECTION('ref_axis',(0.,0.,1.));
#3863=DIRECTION('',(7.77774425693207E-18,0.,-1.));
#3864=DIRECTION('',(-0.0635333619109615,0.997979715186782,0.));
#3865=DIRECTION('center_axis',(0.997979715186782,0.063533361910961,0.));
#3866=DIRECTION('ref_axis',(0.,0.,-1.));
#3867=DIRECTION('',(0.0635333619109615,-0.997979715186782,0.));
#3868=DIRECTION('',(-7.77774425693207E-18,0.,1.));
#3869=DIRECTION('center_axis',(0.,-1.,0.));
#3870=DIRECTION('ref_axis',(-3.21624529935327E-16,0.,1.));
#3871=DIRECTION('center_axis',(0.,1.,0.));
#3872=DIRECTION('ref_axis',(0.,0.,1.));
#3873=DIRECTION('',(0.,-1.,0.));
#3874=DIRECTION('center_axis',(0.,1.,0.));
#3875=DIRECTION('ref_axis',(0.,0.,1.));
#3876=DIRECTION('',(0.,-1.,0.));
#3877=DIRECTION('center_axis',(-1.,0.,-4.07925350989523E-16));
#3878=DIRECTION('ref_axis',(-4.07925350989523E-16,0.,1.));
#3879=DIRECTION('',(3.91608336949942E-16,0.,-1.));
#3880=DIRECTION('',(0.,-1.,0.));
#3881=DIRECTION('',(3.91608336949942E-16,0.,-1.));
#3882=DIRECTION('center_axis',(0.,0.,1.));
#3883=DIRECTION('ref_axis',(1.,0.,0.));
#3884=DIRECTION('',(-1.,0.,0.));
#3885=DIRECTION('',(0.,-1.,0.));
#3886=DIRECTION('',(-1.,0.,0.));
#3887=DIRECTION('center_axis',(1.,0.,-4.07925350989523E-16));
#3888=DIRECTION('ref_axis',(-4.07925350989523E-16,0.,-1.));
#3889=DIRECTION('',(3.91608336949942E-16,0.,1.));
#3890=DIRECTION('',(3.91608336949942E-16,0.,1.));
#3891=DIRECTION('center_axis',(0.,1.,0.));
#3892=DIRECTION('ref_axis',(0.,0.,1.));
#3893=DIRECTION('center_axis',(0.,1.,0.));
#3894=DIRECTION('ref_axis',(0.,0.,1.));
#3895=DIRECTION('',(-0.134182072203336,0.,0.990956695067559));
#3896=DIRECTION('',(0.990956695067559,0.,0.134182072203336));
#3897=DIRECTION('',(-0.0352243074763095,0.,0.999379431528793));
#3898=DIRECTION('',(0.998759248162814,0.0352243074763095,0.0352024483816696));
#3899=DIRECTION('',(-0.012051316852849,0.,0.999927380244242));
#3900=DIRECTION('',(0.999927380244242,0.,0.012051316852849));
#3901=DIRECTION('',(-0.0352243074763103,-5.74085050331075E-17,0.999379431528793));
#3902=DIRECTION('',(0.998759248162814,0.0352243074763094,0.0352024483816704));
#3903=DIRECTION('',(0.698446233568507,0.,0.715662531374926));
#3904=DIRECTION('',(0.715662531374926,0.,-0.698446233568507));
#3905=CARTESIAN_POINT('',(0.,0.,0.));
#3906=CARTESIAN_POINT('',(0.,0.,0.));
#3907=CARTESIAN_POINT('',(0.,0.,0.));
#3908=CARTESIAN_POINT('Origin',(-7.105427357601E-14,49.5625000013656,-6.0924204042587E-14));
#3909=CARTESIAN_POINT('',(104.958734125,0.187500001365581,-6.0924204042587E-14));
#3910=CARTESIAN_POINT('',(104.958734125,-0.0624999986344188,-6.0924204042587E-14));
#3911=CARTESIAN_POINT('',(104.958734125,49.5625000013656,-1.089946703063E-13));
#3912=CARTESIAN_POINT('',(-104.958734125,-0.562499998634419,0.));
#3913=CARTESIAN_POINT('Ctrl Pts',(104.958734125,-0.0624999986344188,-1.28537377788739E-14));
#3914=CARTESIAN_POINT('Ctrl Pts',(104.958734125,-0.124999998634419,43.4753311640868));
#3915=CARTESIAN_POINT('Ctrl Pts',(74.2170326445434,-0.187499998634419,74.2170326445434));
#3916=CARTESIAN_POINT('Ctrl Pts',(43.4753311640869,-0.249999998634419,104.958734125));
#3917=CARTESIAN_POINT('Ctrl Pts',(1.92806066683109E-14,-0.312499998634419,
104.958734125));
#3918=CARTESIAN_POINT('Ctrl Pts',(-43.4753311640868,-0.374999998634419,
104.958734125));
#3919=CARTESIAN_POINT('Ctrl Pts',(-74.2170326445434,-0.437499998634419,
74.2170326445434));
#3920=CARTESIAN_POINT('Ctrl Pts',(-104.958734125,-0.499999998634419,43.4753311640869));
#3921=CARTESIAN_POINT('Ctrl Pts',(-104.958734125,-0.562499998634419,0.));
#3922=CARTESIAN_POINT('',(-104.958734125,-0.312499998634419,0.));
#3923=CARTESIAN_POINT('',(-104.958734125,-0.312499998634419,0.));
#3924=CARTESIAN_POINT('Ctrl Pts',(104.958734125,0.187500001365581,-1.28537377788739E-14));
#3925=CARTESIAN_POINT('Ctrl Pts',(104.958734125,0.125000001365581,43.4753311640868));
#3926=CARTESIAN_POINT('Ctrl Pts',(74.2170326445434,0.0625000013655813,74.2170326445434));
#3927=CARTESIAN_POINT('Ctrl Pts',(43.4753311640869,1.36558125918285E-9,
104.958734125));
#3928=CARTESIAN_POINT('Ctrl Pts',(1.92806066683109E-14,-0.0624999986344188,
104.958734125));
#3929=CARTESIAN_POINT('Ctrl Pts',(-43.4753311640868,-0.124999998634419,
104.958734125));
#3930=CARTESIAN_POINT('Ctrl Pts',(-74.2170326445434,-0.187499998634419,
74.2170326445434));
#3931=CARTESIAN_POINT('Ctrl Pts',(-104.958734125,-0.249999998634419,43.4753311640869));
#3932=CARTESIAN_POINT('Ctrl Pts',(-104.958734125,-0.312499998634419,0.));
#3933=CARTESIAN_POINT('Origin',(-7.105427357601E-14,49.5625000013656,-6.0924204042587E-14));
#3934=CARTESIAN_POINT('',(104.958734125,1.18750000136558,-6.0924204042587E-14));
#3935=CARTESIAN_POINT('',(104.958734125,0.937500001365582,-6.0924204042587E-14));
#3936=CARTESIAN_POINT('',(104.958734125,49.5625000013656,-1.089946703063E-13));
#3937=CARTESIAN_POINT('Ctrl Pts',(104.958734125,0.937500001365582,-1.28537377788739E-14));
#3938=CARTESIAN_POINT('Ctrl Pts',(104.958734125,0.875000001365582,43.4753311640868));
#3939=CARTESIAN_POINT('Ctrl Pts',(74.2170326445434,0.812500001365582,74.2170326445434));
#3940=CARTESIAN_POINT('Ctrl Pts',(43.4753311640869,0.750000001365582,104.958734125));
#3941=CARTESIAN_POINT('Ctrl Pts',(1.92806066683109E-14,0.687500001365582,
104.958734125));
#3942=CARTESIAN_POINT('Ctrl Pts',(-43.4753311640868,0.625000001365582,104.958734125));
#3943=CARTESIAN_POINT('Ctrl Pts',(-74.2170326445434,0.562500001365582,74.2170326445434));
#3944=CARTESIAN_POINT('Ctrl Pts',(-104.958734125,0.500000001365582,43.4753311640869));
#3945=CARTESIAN_POINT('Ctrl Pts',(-104.958734125,0.437500001365582,0.));
#3946=CARTESIAN_POINT('Ctrl Pts',(-104.958734125,0.375000001365582,-43.4753311640868));
#3947=CARTESIAN_POINT('Ctrl Pts',(-74.2170326445434,0.312500001365582,-74.2170326445434));
#3948=CARTESIAN_POINT('Ctrl Pts',(-43.4753311640868,0.250000001365581,-104.958734125));
#3949=CARTESIAN_POINT('Ctrl Pts',(-6.42686888943697E-15,0.187500001365581,
-104.958734125));
#3950=CARTESIAN_POINT('Ctrl Pts',(43.4753311640868,0.125000001365581,-104.958734125));
#3951=CARTESIAN_POINT('Ctrl Pts',(74.2170326445434,0.0625000013655813,-74.2170326445434));
#3952=CARTESIAN_POINT('Ctrl Pts',(104.958734125,1.36558125918285E-9,-43.4753311640868));
#3953=CARTESIAN_POINT('Ctrl Pts',(104.958734125,-0.0624999986344188,-1.28537377788739E-14));
#3954=CARTESIAN_POINT('Ctrl Pts',(104.958734125,1.18750000136558,-1.28537377788739E-14));
#3955=CARTESIAN_POINT('Ctrl Pts',(104.958734125,1.12500000136558,43.4753311640868));
#3956=CARTESIAN_POINT('Ctrl Pts',(74.2170326445434,1.06250000136558,74.2170326445434));
#3957=CARTESIAN_POINT('Ctrl Pts',(43.4753311640869,1.00000000136558,104.958734125));
#3958=CARTESIAN_POINT('Ctrl Pts',(1.92806066683109E-14,0.937500001365582,
104.958734125));
#3959=CARTESIAN_POINT('Ctrl Pts',(-43.4753311640868,0.875000001365582,104.958734125));
#3960=CARTESIAN_POINT('Ctrl Pts',(-74.2170326445434,0.812500001365582,74.2170326445434));
#3961=CARTESIAN_POINT('Ctrl Pts',(-104.958734125,0.750000001365582,43.4753311640869));
#3962=CARTESIAN_POINT('Ctrl Pts',(-104.958734125,0.687500001365582,0.));
#3963=CARTESIAN_POINT('Ctrl Pts',(-104.958734125,0.625000001365582,-43.4753311640868));
#3964=CARTESIAN_POINT('Ctrl Pts',(-74.2170326445434,0.562500001365582,-74.2170326445434));
#3965=CARTESIAN_POINT('Ctrl Pts',(-43.4753311640868,0.500000001365582,-104.958734125));
#3966=CARTESIAN_POINT('Ctrl Pts',(-6.42686888943697E-15,0.437500001365582,
-104.958734125));
#3967=CARTESIAN_POINT('Ctrl Pts',(43.4753311640868,0.375000001365582,-104.958734125));
#3968=CARTESIAN_POINT('Ctrl Pts',(74.2170326445434,0.312500001365582,-74.2170326445434));
#3969=CARTESIAN_POINT('Ctrl Pts',(104.958734125,0.250000001365581,-43.4753311640868));
#3970=CARTESIAN_POINT('Ctrl Pts',(104.958734125,0.187500001365581,-1.28537377788739E-14));
#3971=CARTESIAN_POINT('Origin',(-7.105427357601E-14,49.5625000013656,-6.0924204042587E-14));
#3972=CARTESIAN_POINT('',(104.958734125,2.18750000136558,-6.0924204042587E-14));
#3973=CARTESIAN_POINT('',(104.958734125,1.93750000136558,-6.0924204042587E-14));
#3974=CARTESIAN_POINT('',(104.958734125,49.5625000013656,-1.089946703063E-13));
#3975=CARTESIAN_POINT('Ctrl Pts',(104.958734125,1.93750000136558,-1.28537377788739E-14));
#3976=CARTESIAN_POINT('Ctrl Pts',(104.958734125,1.87500000136558,43.4753311640868));
#3977=CARTESIAN_POINT('Ctrl Pts',(74.2170326445434,1.81250000136558,74.2170326445434));
#3978=CARTESIAN_POINT('Ctrl Pts',(43.4753311640869,1.75000000136558,104.958734125));
#3979=CARTESIAN_POINT('Ctrl Pts',(1.92806066683109E-14,1.68750000136558,
104.958734125));
#3980=CARTESIAN_POINT('Ctrl Pts',(-43.4753311640868,1.62500000136558,104.958734125));
#3981=CARTESIAN_POINT('Ctrl Pts',(-74.2170326445434,1.56250000136558,74.2170326445434));
#3982=CARTESIAN_POINT('Ctrl Pts',(-104.958734125,1.50000000136558,43.4753311640869));
#3983=CARTESIAN_POINT('Ctrl Pts',(-104.958734125,1.43750000136558,0.));
#3984=CARTESIAN_POINT('Ctrl Pts',(-104.958734125,1.37500000136558,-43.4753311640868));
#3985=CARTESIAN_POINT('Ctrl Pts',(-74.2170326445434,1.31250000136558,-74.2170326445434));
#3986=CARTESIAN_POINT('Ctrl Pts',(-43.4753311640868,1.25000000136558,-104.958734125));
#3987=CARTESIAN_POINT('Ctrl Pts',(-6.42686888943697E-15,1.18750000136558,
-104.958734125));
#3988=CARTESIAN_POINT('Ctrl Pts',(43.4753311640868,1.12500000136558,-104.958734125));
#3989=CARTESIAN_POINT('Ctrl Pts',(74.2170326445434,1.06250000136558,-74.2170326445434));
#3990=CARTESIAN_POINT('Ctrl Pts',(104.958734125,1.00000000136558,-43.4753311640868));
#3991=CARTESIAN_POINT('Ctrl Pts',(104.958734125,0.937500001365582,-1.28537377788739E-14));
#3992=CARTESIAN_POINT('Ctrl Pts',(104.958734125,2.18750000136558,-1.28537377788739E-14));
#3993=CARTESIAN_POINT('Ctrl Pts',(104.958734125,2.12500000136558,43.4753311640868));
#3994=CARTESIAN_POINT('Ctrl Pts',(74.2170326445434,2.06250000136558,74.2170326445434));
#3995=CARTESIAN_POINT('Ctrl Pts',(43.4753311640869,2.00000000136558,104.958734125));
#3996=CARTESIAN_POINT('Ctrl Pts',(1.92806066683109E-14,1.93750000136558,
104.958734125));
#3997=CARTESIAN_POINT('Ctrl Pts',(-43.4753311640868,1.87500000136558,104.958734125));
#3998=CARTESIAN_POINT('Ctrl Pts',(-74.2170326445434,1.81250000136558,74.2170326445434));
#3999=CARTESIAN_POINT('Ctrl Pts',(-104.958734125,1.75000000136558,43.4753311640869));
#4000=CARTESIAN_POINT('Ctrl Pts',(-104.958734125,1.68750000136558,0.));
#4001=CARTESIAN_POINT('Ctrl Pts',(-104.958734125,1.62500000136558,-43.4753311640868));
#4002=CARTESIAN_POINT('Ctrl Pts',(-74.2170326445434,1.56250000136558,-74.2170326445434));
#4003=CARTESIAN_POINT('Ctrl Pts',(-43.4753311640868,1.50000000136558,-104.958734125));
#4004=CARTESIAN_POINT('Ctrl Pts',(-6.42686888943697E-15,1.43750000136558,
-104.958734125));
#4005=CARTESIAN_POINT('Ctrl Pts',(43.4753311640868,1.37500000136558,-104.958734125));
#4006=CARTESIAN_POINT('Ctrl Pts',(74.2170326445434,1.31250000136558,-74.2170326445434));
#4007=CARTESIAN_POINT('Ctrl Pts',(104.958734125,1.25000000136558,-43.4753311640868));
#4008=CARTESIAN_POINT('Ctrl Pts',(104.958734125,1.18750000136558,-1.28537377788739E-14));
#4009=CARTESIAN_POINT('Origin',(-7.105427357601E-14,49.5625000013656,-6.0924204042587E-14));
#4010=CARTESIAN_POINT('',(104.958734125,3.18750000136558,-6.0924204042587E-14));
#4011=CARTESIAN_POINT('',(104.958734125,2.93750000136558,-6.0924204042587E-14));
#4012=CARTESIAN_POINT('',(104.958734125,49.5625000013656,-1.089946703063E-13));
#4013=CARTESIAN_POINT('Ctrl Pts',(104.958734125,2.93750000136558,-1.28537377788739E-14));
#4014=CARTESIAN_POINT('Ctrl Pts',(104.958734125,2.87500000136558,43.4753311640868));
#4015=CARTESIAN_POINT('Ctrl Pts',(74.2170326445434,2.81250000136558,74.2170326445434));
#4016=CARTESIAN_POINT('Ctrl Pts',(43.4753311640869,2.75000000136558,104.958734125));
#4017=CARTESIAN_POINT('Ctrl Pts',(1.92806066683109E-14,2.68750000136558,
104.958734125));
#4018=CARTESIAN_POINT('Ctrl Pts',(-43.4753311640868,2.62500000136558,104.958734125));
#4019=CARTESIAN_POINT('Ctrl Pts',(-74.2170326445434,2.56250000136558,74.2170326445434));
#4020=CARTESIAN_POINT('Ctrl Pts',(-104.958734125,2.50000000136558,43.4753311640869));
#4021=CARTESIAN_POINT('Ctrl Pts',(-104.958734125,2.43750000136558,0.));
#4022=CARTESIAN_POINT('Ctrl Pts',(-104.958734125,2.37500000136558,-43.4753311640868));
#4023=CARTESIAN_POINT('Ctrl Pts',(-74.2170326445434,2.31250000136558,-74.2170326445434));
#4024=CARTESIAN_POINT('Ctrl Pts',(-43.4753311640868,2.25000000136558,-104.958734125));
#4025=CARTESIAN_POINT('Ctrl Pts',(-6.42686888943697E-15,2.18750000136558,
-104.958734125));
#4026=CARTESIAN_POINT('Ctrl Pts',(43.4753311640868,2.12500000136558,-104.958734125));
#4027=CARTESIAN_POINT('Ctrl Pts',(74.2170326445434,2.06250000136558,-74.2170326445434));
#4028=CARTESIAN_POINT('Ctrl Pts',(104.958734125,2.00000000136558,-43.4753311640868));
#4029=CARTESIAN_POINT('Ctrl Pts',(104.958734125,1.93750000136558,-1.28537377788739E-14));
#4030=CARTESIAN_POINT('Ctrl Pts',(104.958734125,3.18750000136558,-1.28537377788739E-14));
#4031=CARTESIAN_POINT('Ctrl Pts',(104.958734125,3.12500000136558,43.4753311640868));
#4032=CARTESIAN_POINT('Ctrl Pts',(74.2170326445434,3.06250000136558,74.2170326445434));
#4033=CARTESIAN_POINT('Ctrl Pts',(43.4753311640869,3.00000000136558,104.958734125));
#4034=CARTESIAN_POINT('Ctrl Pts',(1.92806066683109E-14,2.93750000136558,
104.958734125));
#4035=CARTESIAN_POINT('Ctrl Pts',(-43.4753311640868,2.87500000136558,104.958734125));
#4036=CARTESIAN_POINT('Ctrl Pts',(-74.2170326445434,2.81250000136558,74.2170326445434));
#4037=CARTESIAN_POINT('Ctrl Pts',(-104.958734125,2.75000000136558,43.4753311640869));
#4038=CARTESIAN_POINT('Ctrl Pts',(-104.958734125,2.68750000136558,0.));
#4039=CARTESIAN_POINT('Ctrl Pts',(-104.958734125,2.62500000136558,-43.4753311640868));
#4040=CARTESIAN_POINT('Ctrl Pts',(-74.2170326445434,2.56250000136558,-74.2170326445434));
#4041=CARTESIAN_POINT('Ctrl Pts',(-43.4753311640868,2.50000000136558,-104.958734125));
#4042=CARTESIAN_POINT('Ctrl Pts',(-6.42686888943697E-15,2.43750000136558,
-104.958734125));
#4043=CARTESIAN_POINT('Ctrl Pts',(43.4753311640868,2.37500000136558,-104.958734125));
#4044=CARTESIAN_POINT('Ctrl Pts',(74.2170326445434,2.31250000136558,-74.2170326445434));
#4045=CARTESIAN_POINT('Ctrl Pts',(104.958734125,2.25000000136558,-43.4753311640868));
#4046=CARTESIAN_POINT('Ctrl Pts',(104.958734125,2.18750000136558,-1.28537377788739E-14));
#4047=CARTESIAN_POINT('Origin',(-7.105427357601E-14,49.5625000013656,-6.0924204042587E-14));
#4048=CARTESIAN_POINT('',(104.958734125,4.18750000136558,-6.0924204042587E-14));
#4049=CARTESIAN_POINT('',(104.958734125,3.93750000136558,-6.0924204042587E-14));
#4050=CARTESIAN_POINT('',(104.958734125,49.5625000013656,-1.089946703063E-13));
#4051=CARTESIAN_POINT('Ctrl Pts',(104.958734125,3.93750000136558,-1.28537377788739E-14));
#4052=CARTESIAN_POINT('Ctrl Pts',(104.958734125,3.87500000136558,43.4753311640868));
#4053=CARTESIAN_POINT('Ctrl Pts',(74.2170326445434,3.81250000136558,74.2170326445434));
#4054=CARTESIAN_POINT('Ctrl Pts',(43.4753311640869,3.75000000136558,104.958734125));
#4055=CARTESIAN_POINT('Ctrl Pts',(1.92806066683109E-14,3.68750000136558,
104.958734125));
#4056=CARTESIAN_POINT('Ctrl Pts',(-43.4753311640868,3.62500000136558,104.958734125));
#4057=CARTESIAN_POINT('Ctrl Pts',(-74.2170326445434,3.56250000136558,74.2170326445434));
#4058=CARTESIAN_POINT('Ctrl Pts',(-104.958734125,3.50000000136558,43.4753311640869));
#4059=CARTESIAN_POINT('Ctrl Pts',(-104.958734125,3.43750000136558,0.));
#4060=CARTESIAN_POINT('Ctrl Pts',(-104.958734125,3.37500000136558,-43.4753311640868));
#4061=CARTESIAN_POINT('Ctrl Pts',(-74.2170326445434,3.31250000136558,-74.2170326445434));
#4062=CARTESIAN_POINT('Ctrl Pts',(-43.4753311640868,3.25000000136558,-104.958734125));
#4063=CARTESIAN_POINT('Ctrl Pts',(-6.42686888943697E-15,3.18750000136558,
-104.958734125));
#4064=CARTESIAN_POINT('Ctrl Pts',(43.4753311640868,3.12500000136558,-104.958734125));
#4065=CARTESIAN_POINT('Ctrl Pts',(74.2170326445434,3.06250000136558,-74.2170326445434));
#4066=CARTESIAN_POINT('Ctrl Pts',(104.958734125,3.00000000136558,-43.4753311640868));
#4067=CARTESIAN_POINT('Ctrl Pts',(104.958734125,2.93750000136558,-1.28537377788739E-14));
#4068=CARTESIAN_POINT('Ctrl Pts',(104.958734125,4.18750000136558,-1.28537377788739E-14));
#4069=CARTESIAN_POINT('Ctrl Pts',(104.958734125,4.12500000136558,43.4753311640868));
#4070=CARTESIAN_POINT('Ctrl Pts',(74.2170326445434,4.06250000136558,74.2170326445434));
#4071=CARTESIAN_POINT('Ctrl Pts',(43.4753311640869,4.00000000136558,104.958734125));
#4072=CARTESIAN_POINT('Ctrl Pts',(1.92806066683109E-14,3.93750000136558,
104.958734125));
#4073=CARTESIAN_POINT('Ctrl Pts',(-43.4753311640868,3.87500000136558,104.958734125));
#4074=CARTESIAN_POINT('Ctrl Pts',(-74.2170326445434,3.81250000136558,74.2170326445434));
#4075=CARTESIAN_POINT('Ctrl Pts',(-104.958734125,3.75000000136558,43.4753311640869));
#4076=CARTESIAN_POINT('Ctrl Pts',(-104.958734125,3.68750000136558,0.));
#4077=CARTESIAN_POINT('Ctrl Pts',(-104.958734125,3.62500000136558,-43.4753311640868));
#4078=CARTESIAN_POINT('Ctrl Pts',(-74.2170326445434,3.56250000136558,-74.2170326445434));
#4079=CARTESIAN_POINT('Ctrl Pts',(-43.4753311640868,3.50000000136558,-104.958734125));
#4080=CARTESIAN_POINT('Ctrl Pts',(-6.42686888943697E-15,3.43750000136558,
-104.958734125));
#4081=CARTESIAN_POINT('Ctrl Pts',(43.4753311640868,3.37500000136558,-104.958734125));
#4082=CARTESIAN_POINT('Ctrl Pts',(74.2170326445434,3.31250000136558,-74.2170326445434));
#4083=CARTESIAN_POINT('Ctrl Pts',(104.958734125,3.25000000136558,-43.4753311640868));
#4084=CARTESIAN_POINT('Ctrl Pts',(104.958734125,3.18750000136558,-1.28537377788739E-14));
#4085=CARTESIAN_POINT('Origin',(-7.105427357601E-14,49.5625000013656,-6.0924204042587E-14));
#4086=CARTESIAN_POINT('',(104.958734125,5.18750000136559,-6.0924204042587E-14));
#4087=CARTESIAN_POINT('',(104.958734125,4.93750000136559,-6.0924204042587E-14));
#4088=CARTESIAN_POINT('',(104.958734125,49.5625000013656,-1.089946703063E-13));
#4089=CARTESIAN_POINT('Ctrl Pts',(104.958734125,4.93750000136559,-1.28537377788739E-14));
#4090=CARTESIAN_POINT('Ctrl Pts',(104.958734125,4.87500000136559,43.4753311640868));
#4091=CARTESIAN_POINT('Ctrl Pts',(74.2170326445434,4.81250000136559,74.2170326445434));
#4092=CARTESIAN_POINT('Ctrl Pts',(43.4753311640869,4.75000000136558,104.958734125));
#4093=CARTESIAN_POINT('Ctrl Pts',(1.92806066683109E-14,4.68750000136558,
104.958734125));
#4094=CARTESIAN_POINT('Ctrl Pts',(-43.4753311640868,4.62500000136559,104.958734125));
#4095=CARTESIAN_POINT('Ctrl Pts',(-74.2170326445434,4.56250000136558,74.2170326445434));
#4096=CARTESIAN_POINT('Ctrl Pts',(-104.958734125,4.50000000136558,43.4753311640869));
#4097=CARTESIAN_POINT('Ctrl Pts',(-104.958734125,4.43750000136558,0.));
#4098=CARTESIAN_POINT('Ctrl Pts',(-104.958734125,4.37500000136558,-43.4753311640868));
#4099=CARTESIAN_POINT('Ctrl Pts',(-74.2170326445434,4.31250000136558,-74.2170326445434));
#4100=CARTESIAN_POINT('Ctrl Pts',(-43.4753311640868,4.25000000136558,-104.958734125));
#4101=CARTESIAN_POINT('Ctrl Pts',(-6.42686888943697E-15,4.18750000136558,
-104.958734125));
#4102=CARTESIAN_POINT('Ctrl Pts',(43.4753311640868,4.12500000136558,-104.958734125));
#4103=CARTESIAN_POINT('Ctrl Pts',(74.2170326445434,4.06250000136558,-74.2170326445434));
#4104=CARTESIAN_POINT('Ctrl Pts',(104.958734125,4.00000000136558,-43.4753311640868));
#4105=CARTESIAN_POINT('Ctrl Pts',(104.958734125,3.93750000136558,-1.28537377788739E-14));
#4106=CARTESIAN_POINT('Ctrl Pts',(104.958734125,5.18750000136559,-1.28537377788739E-14));
#4107=CARTESIAN_POINT('Ctrl Pts',(104.958734125,5.12500000136559,43.4753311640868));
#4108=CARTESIAN_POINT('Ctrl Pts',(74.2170326445434,5.06250000136559,74.2170326445434));
#4109=CARTESIAN_POINT('Ctrl Pts',(43.4753311640869,5.00000000136558,104.958734125));
#4110=CARTESIAN_POINT('Ctrl Pts',(1.92806066683109E-14,4.93750000136559,
104.958734125));
#4111=CARTESIAN_POINT('Ctrl Pts',(-43.4753311640868,4.87500000136559,104.958734125));
#4112=CARTESIAN_POINT('Ctrl Pts',(-74.2170326445434,4.81250000136559,74.2170326445434));
#4113=CARTESIAN_POINT('Ctrl Pts',(-104.958734125,4.75000000136558,43.4753311640869));
#4114=CARTESIAN_POINT('Ctrl Pts',(-104.958734125,4.68750000136558,0.));
#4115=CARTESIAN_POINT('Ctrl Pts',(-104.958734125,4.62500000136559,-43.4753311640868));
#4116=CARTESIAN_POINT('Ctrl Pts',(-74.2170326445434,4.56250000136558,-74.2170326445434));
#4117=CARTESIAN_POINT('Ctrl Pts',(-43.4753311640868,4.50000000136558,-104.958734125));
#4118=CARTESIAN_POINT('Ctrl Pts',(-6.42686888943697E-15,4.43750000136558,
-104.958734125));
#4119=CARTESIAN_POINT('Ctrl Pts',(43.4753311640868,4.37500000136558,-104.958734125));
#4120=CARTESIAN_POINT('Ctrl Pts',(74.2170326445434,4.31250000136558,-74.2170326445434));
#4121=CARTESIAN_POINT('Ctrl Pts',(104.958734125,4.25000000136558,-43.4753311640868));
#4122=CARTESIAN_POINT('Ctrl Pts',(104.958734125,4.18750000136558,-1.28537377788739E-14));
#4123=CARTESIAN_POINT('Origin',(-7.105427357601E-14,49.5625000013656,-6.0924204042587E-14));
#4124=CARTESIAN_POINT('',(104.958734125,6.18750000136558,-6.0924204042587E-14));
#4125=CARTESIAN_POINT('',(104.958734125,5.93750000136558,-6.0924204042587E-14));
#4126=CARTESIAN_POINT('',(104.958734125,49.5625000013656,-1.089946703063E-13));
#4127=CARTESIAN_POINT('Ctrl Pts',(104.958734125,5.93750000136558,-1.28537377788739E-14));
#4128=CARTESIAN_POINT('Ctrl Pts',(104.958734125,5.87500000136558,43.4753311640868));
#4129=CARTESIAN_POINT('Ctrl Pts',(74.2170326445434,5.81250000136558,74.2170326445434));
#4130=CARTESIAN_POINT('Ctrl Pts',(43.4753311640869,5.75000000136558,104.958734125));
#4131=CARTESIAN_POINT('Ctrl Pts',(1.92806066683109E-14,5.68750000136558,
104.958734125));
#4132=CARTESIAN_POINT('Ctrl Pts',(-43.4753311640868,5.62500000136558,104.958734125));
#4133=CARTESIAN_POINT('Ctrl Pts',(-74.2170326445434,5.56250000136558,74.2170326445434));
#4134=CARTESIAN_POINT('Ctrl Pts',(-104.958734125,5.50000000136558,43.4753311640869));
#4135=CARTESIAN_POINT('Ctrl Pts',(-104.958734125,5.43750000136559,0.));
#4136=CARTESIAN_POINT('Ctrl Pts',(-104.958734125,5.37500000136559,-43.4753311640868));
#4137=CARTESIAN_POINT('Ctrl Pts',(-74.2170326445434,5.31250000136558,-74.2170326445434));
#4138=CARTESIAN_POINT('Ctrl Pts',(-43.4753311640868,5.25000000136559,-104.958734125));
#4139=CARTESIAN_POINT('Ctrl Pts',(-6.42686888943697E-15,5.18750000136559,
-104.958734125));
#4140=CARTESIAN_POINT('Ctrl Pts',(43.4753311640868,5.12500000136559,-104.958734125));
#4141=CARTESIAN_POINT('Ctrl Pts',(74.2170326445434,5.06250000136559,-74.2170326445434));
#4142=CARTESIAN_POINT('Ctrl Pts',(104.958734125,5.00000000136558,-43.4753311640868));
#4143=CARTESIAN_POINT('Ctrl Pts',(104.958734125,4.93750000136559,-1.28537377788739E-14));
#4144=CARTESIAN_POINT('Ctrl Pts',(104.958734125,6.18750000136558,-1.28537377788739E-14));
#4145=CARTESIAN_POINT('Ctrl Pts',(104.958734125,6.12500000136558,43.4753311640868));
#4146=CARTESIAN_POINT('Ctrl Pts',(74.2170326445434,6.06250000136558,74.2170326445434));
#4147=CARTESIAN_POINT('Ctrl Pts',(43.4753311640869,6.00000000136558,104.958734125));
#4148=CARTESIAN_POINT('Ctrl Pts',(1.92806066683109E-14,5.93750000136558,
104.958734125));
#4149=CARTESIAN_POINT('Ctrl Pts',(-43.4753311640868,5.87500000136558,104.958734125));
#4150=CARTESIAN_POINT('Ctrl Pts',(-74.2170326445434,5.81250000136558,74.2170326445434));
#4151=CARTESIAN_POINT('Ctrl Pts',(-104.958734125,5.75000000136558,43.4753311640869));
#4152=CARTESIAN_POINT('Ctrl Pts',(-104.958734125,5.68750000136559,0.));
#4153=CARTESIAN_POINT('Ctrl Pts',(-104.958734125,5.62500000136559,-43.4753311640868));
#4154=CARTESIAN_POINT('Ctrl Pts',(-74.2170326445434,5.56250000136559,-74.2170326445434));
#4155=CARTESIAN_POINT('Ctrl Pts',(-43.4753311640868,5.50000000136559,-104.958734125));
#4156=CARTESIAN_POINT('Ctrl Pts',(-6.42686888943697E-15,5.43750000136559,
-104.958734125));
#4157=CARTESIAN_POINT('Ctrl Pts',(43.4753311640868,5.37500000136559,-104.958734125));
#4158=CARTESIAN_POINT('Ctrl Pts',(74.2170326445434,5.31250000136558,-74.2170326445434));
#4159=CARTESIAN_POINT('Ctrl Pts',(104.958734125,5.25000000136559,-43.4753311640868));
#4160=CARTESIAN_POINT('Ctrl Pts',(104.958734125,5.18750000136559,-1.28537377788739E-14));
#4161=CARTESIAN_POINT('Origin',(-7.105427357601E-14,49.5625000013656,-6.0924204042587E-14));
#4162=CARTESIAN_POINT('',(104.958734125,7.18750000136558,-6.0924204042587E-14));
#4163=CARTESIAN_POINT('',(104.958734125,6.93750000136558,-6.0924204042587E-14));
#4164=CARTESIAN_POINT('',(104.958734125,49.5625000013656,-1.089946703063E-13));
#4165=CARTESIAN_POINT('Ctrl Pts',(104.958734125,6.93750000136558,-1.28537377788739E-14));
#4166=CARTESIAN_POINT('Ctrl Pts',(104.958734125,6.87500000136558,43.4753311640868));
#4167=CARTESIAN_POINT('Ctrl Pts',(74.2170326445434,6.81250000136558,74.2170326445434));
#4168=CARTESIAN_POINT('Ctrl Pts',(43.4753311640869,6.75000000136558,104.958734125));
#4169=CARTESIAN_POINT('Ctrl Pts',(1.92806066683109E-14,6.68750000136558,
104.958734125));
#4170=CARTESIAN_POINT('Ctrl Pts',(-43.4753311640868,6.62500000136558,104.958734125));
#4171=CARTESIAN_POINT('Ctrl Pts',(-74.2170326445434,6.56250000136558,74.2170326445434));
#4172=CARTESIAN_POINT('Ctrl Pts',(-104.958734125,6.50000000136558,43.4753311640869));
#4173=CARTESIAN_POINT('Ctrl Pts',(-104.958734125,6.43750000136558,0.));
#4174=CARTESIAN_POINT('Ctrl Pts',(-104.958734125,6.37500000136558,-43.4753311640868));
#4175=CARTESIAN_POINT('Ctrl Pts',(-74.2170326445434,6.31250000136558,-74.2170326445434));
#4176=CARTESIAN_POINT('Ctrl Pts',(-43.4753311640868,6.25000000136558,-104.958734125));
#4177=CARTESIAN_POINT('Ctrl Pts',(-6.42686888943697E-15,6.18750000136558,
-104.958734125));
#4178=CARTESIAN_POINT('Ctrl Pts',(43.4753311640868,6.12500000136558,-104.958734125));
#4179=CARTESIAN_POINT('Ctrl Pts',(74.2170326445434,6.06250000136558,-74.2170326445434));
#4180=CARTESIAN_POINT('Ctrl Pts',(104.958734125,6.00000000136558,-43.4753311640868));
#4181=CARTESIAN_POINT('Ctrl Pts',(104.958734125,5.93750000136558,-1.28537377788739E-14));
#4182=CARTESIAN_POINT('Ctrl Pts',(104.958734125,7.18750000136558,-1.28537377788739E-14));
#4183=CARTESIAN_POINT('Ctrl Pts',(104.958734125,7.12500000136558,43.4753311640868));
#4184=CARTESIAN_POINT('Ctrl Pts',(74.2170326445434,7.06250000136558,74.2170326445434));
#4185=CARTESIAN_POINT('Ctrl Pts',(43.4753311640869,7.00000000136558,104.958734125));
#4186=CARTESIAN_POINT('Ctrl Pts',(1.92806066683109E-14,6.93750000136558,
104.958734125));
#4187=CARTESIAN_POINT('Ctrl Pts',(-43.4753311640868,6.87500000136558,104.958734125));
#4188=CARTESIAN_POINT('Ctrl Pts',(-74.2170326445434,6.81250000136558,74.2170326445434));
#4189=CARTESIAN_POINT('Ctrl Pts',(-104.958734125,6.75000000136558,43.4753311640869));
#4190=CARTESIAN_POINT('Ctrl Pts',(-104.958734125,6.68750000136558,0.));
#4191=CARTESIAN_POINT('Ctrl Pts',(-104.958734125,6.62500000136558,-43.4753311640868));
#4192=CARTESIAN_POINT('Ctrl Pts',(-74.2170326445434,6.56250000136558,-74.2170326445434));
#4193=CARTESIAN_POINT('Ctrl Pts',(-43.4753311640868,6.50000000136558,-104.958734125));
#4194=CARTESIAN_POINT('Ctrl Pts',(-6.42686888943697E-15,6.43750000136558,
-104.958734125));
#4195=CARTESIAN_POINT('Ctrl Pts',(43.4753311640868,6.37500000136558,-104.958734125));
#4196=CARTESIAN_POINT('Ctrl Pts',(74.2170326445434,6.31250000136558,-74.2170326445434));
#4197=CARTESIAN_POINT('Ctrl Pts',(104.958734125,6.25000000136558,-43.4753311640868));
#4198=CARTESIAN_POINT('Ctrl Pts',(104.958734125,6.18750000136558,-1.28537377788739E-14));
#4199=CARTESIAN_POINT('Origin',(-7.105427357601E-14,49.5625000013656,-6.0924204042587E-14));
#4200=CARTESIAN_POINT('',(104.958734125,8.18750000136558,-6.0924204042587E-14));
#4201=CARTESIAN_POINT('',(104.958734125,7.93750000136558,-6.0924204042587E-14));
#4202=CARTESIAN_POINT('',(104.958734125,49.5625000013656,-1.089946703063E-13));
#4203=CARTESIAN_POINT('Ctrl Pts',(104.958734125,7.93750000136558,-1.28537377788739E-14));
#4204=CARTESIAN_POINT('Ctrl Pts',(104.958734125,7.87500000136558,43.4753311640868));
#4205=CARTESIAN_POINT('Ctrl Pts',(74.2170326445434,7.81250000136558,74.2170326445434));
#4206=CARTESIAN_POINT('Ctrl Pts',(43.4753311640869,7.75000000136558,104.958734125));
#4207=CARTESIAN_POINT('Ctrl Pts',(1.92806066683109E-14,7.68750000136558,
104.958734125));
#4208=CARTESIAN_POINT('Ctrl Pts',(-43.4753311640868,7.62500000136558,104.958734125));
#4209=CARTESIAN_POINT('Ctrl Pts',(-74.2170326445434,7.56250000136558,74.2170326445434));
#4210=CARTESIAN_POINT('Ctrl Pts',(-104.958734125,7.50000000136558,43.4753311640869));
#4211=CARTESIAN_POINT('Ctrl Pts',(-104.958734125,7.43750000136558,0.));
#4212=CARTESIAN_POINT('Ctrl Pts',(-104.958734125,7.37500000136558,-43.4753311640868));
#4213=CARTESIAN_POINT('Ctrl Pts',(-74.2170326445434,7.31250000136558,-74.2170326445434));
#4214=CARTESIAN_POINT('Ctrl Pts',(-43.4753311640868,7.25000000136558,-104.958734125));
#4215=CARTESIAN_POINT('Ctrl Pts',(-6.42686888943697E-15,7.18750000136558,
-104.958734125));
#4216=CARTESIAN_POINT('Ctrl Pts',(43.4753311640868,7.12500000136558,-104.958734125));
#4217=CARTESIAN_POINT('Ctrl Pts',(74.2170326445434,7.06250000136558,-74.2170326445434));
#4218=CARTESIAN_POINT('Ctrl Pts',(104.958734125,7.00000000136558,-43.4753311640868));
#4219=CARTESIAN_POINT('Ctrl Pts',(104.958734125,6.93750000136558,-1.28537377788739E-14));
#4220=CARTESIAN_POINT('Ctrl Pts',(104.958734125,8.18750000136558,-1.28537377788739E-14));
#4221=CARTESIAN_POINT('Ctrl Pts',(104.958734125,8.12500000136558,43.4753311640868));
#4222=CARTESIAN_POINT('Ctrl Pts',(74.2170326445434,8.06250000136558,74.2170326445434));
#4223=CARTESIAN_POINT('Ctrl Pts',(43.4753311640869,8.00000000136558,104.958734125));
#4224=CARTESIAN_POINT('Ctrl Pts',(1.92806066683109E-14,7.93750000136558,
104.958734125));
#4225=CARTESIAN_POINT('Ctrl Pts',(-43.4753311640868,7.87500000136558,104.958734125));
#4226=CARTESIAN_POINT('Ctrl Pts',(-74.2170326445434,7.81250000136558,74.2170326445434));
#4227=CARTESIAN_POINT('Ctrl Pts',(-104.958734125,7.75000000136558,43.4753311640869));
#4228=CARTESIAN_POINT('Ctrl Pts',(-104.958734125,7.68750000136558,0.));
#4229=CARTESIAN_POINT('Ctrl Pts',(-104.958734125,7.62500000136558,-43.4753311640868));
#4230=CARTESIAN_POINT('Ctrl Pts',(-74.2170326445434,7.56250000136558,-74.2170326445434));
#4231=CARTESIAN_POINT('Ctrl Pts',(-43.4753311640868,7.50000000136558,-104.958734125));
#4232=CARTESIAN_POINT('Ctrl Pts',(-6.42686888943697E-15,7.43750000136558,
-104.958734125));
#4233=CARTESIAN_POINT('Ctrl Pts',(43.4753311640868,7.37500000136558,-104.958734125));
#4234=CARTESIAN_POINT('Ctrl Pts',(74.2170326445434,7.31250000136558,-74.2170326445434));
#4235=CARTESIAN_POINT('Ctrl Pts',(104.958734125,7.25000000136558,-43.4753311640868));
#4236=CARTESIAN_POINT('Ctrl Pts',(104.958734125,7.18750000136558,-1.28537377788739E-14));
#4237=CARTESIAN_POINT('Origin',(-7.105427357601E-14,49.5625000013656,-6.0924204042587E-14));
#4238=CARTESIAN_POINT('',(104.958734125,9.18750000136558,-6.0924204042587E-14));
#4239=CARTESIAN_POINT('',(104.958734125,8.93750000136558,-6.0924204042587E-14));
#4240=CARTESIAN_POINT('',(104.958734125,49.5625000013656,-1.089946703063E-13));
#4241=CARTESIAN_POINT('Ctrl Pts',(104.958734125,8.93750000136558,-1.28537377788739E-14));
#4242=CARTESIAN_POINT('Ctrl Pts',(104.958734125,8.87500000136558,43.4753311640868));
#4243=CARTESIAN_POINT('Ctrl Pts',(74.2170326445434,8.81250000136558,74.2170326445434));
#4244=CARTESIAN_POINT('Ctrl Pts',(43.4753311640869,8.75000000136558,104.958734125));
#4245=CARTESIAN_POINT('Ctrl Pts',(1.92806066683109E-14,8.68750000136558,
104.958734125));
#4246=CARTESIAN_POINT('Ctrl Pts',(-43.4753311640868,8.62500000136558,104.958734125));
#4247=CARTESIAN_POINT('Ctrl Pts',(-74.2170326445434,8.56250000136558,74.2170326445434));
#4248=CARTESIAN_POINT('Ctrl Pts',(-104.958734125,8.50000000136558,43.4753311640869));
#4249=CARTESIAN_POINT('Ctrl Pts',(-104.958734125,8.43750000136558,0.));
#4250=CARTESIAN_POINT('Ctrl Pts',(-104.958734125,8.37500000136558,-43.4753311640868));
#4251=CARTESIAN_POINT('Ctrl Pts',(-74.2170326445434,8.31250000136558,-74.2170326445434));
#4252=CARTESIAN_POINT('Ctrl Pts',(-43.4753311640868,8.25000000136558,-104.958734125));
#4253=CARTESIAN_POINT('Ctrl Pts',(-6.42686888943697E-15,8.18750000136558,
-104.958734125));
#4254=CARTESIAN_POINT('Ctrl Pts',(43.4753311640868,8.12500000136558,-104.958734125));
#4255=CARTESIAN_POINT('Ctrl Pts',(74.2170326445434,8.06250000136558,-74.2170326445434));
#4256=CARTESIAN_POINT('Ctrl Pts',(104.958734125,8.00000000136558,-43.4753311640868));
#4257=CARTESIAN_POINT('Ctrl Pts',(104.958734125,7.93750000136558,-1.28537377788739E-14));
#4258=CARTESIAN_POINT('Ctrl Pts',(104.958734125,9.18750000136558,-1.28537377788739E-14));
#4259=CARTESIAN_POINT('Ctrl Pts',(104.958734125,9.12500000136558,43.4753311640868));
#4260=CARTESIAN_POINT('Ctrl Pts',(74.2170326445434,9.06250000136558,74.2170326445434));
#4261=CARTESIAN_POINT('Ctrl Pts',(43.4753311640869,9.00000000136558,104.958734125));
#4262=CARTESIAN_POINT('Ctrl Pts',(1.92806066683109E-14,8.93750000136558,
104.958734125));
#4263=CARTESIAN_POINT('Ctrl Pts',(-43.4753311640868,8.87500000136558,104.958734125));
#4264=CARTESIAN_POINT('Ctrl Pts',(-74.2170326445434,8.81250000136558,74.2170326445434));
#4265=CARTESIAN_POINT('Ctrl Pts',(-104.958734125,8.75000000136558,43.4753311640869));
#4266=CARTESIAN_POINT('Ctrl Pts',(-104.958734125,8.68750000136558,0.));
#4267=CARTESIAN_POINT('Ctrl Pts',(-104.958734125,8.62500000136558,-43.4753311640868));
#4268=CARTESIAN_POINT('Ctrl Pts',(-74.2170326445434,8.56250000136558,-74.2170326445434));
#4269=CARTESIAN_POINT('Ctrl Pts',(-43.4753311640868,8.50000000136558,-104.958734125));
#4270=CARTESIAN_POINT('Ctrl Pts',(-6.42686888943697E-15,8.43750000136558,
-104.958734125));
#4271=CARTESIAN_POINT('Ctrl Pts',(43.4753311640868,8.37500000136558,-104.958734125));
#4272=CARTESIAN_POINT('Ctrl Pts',(74.2170326445434,8.31250000136558,-74.2170326445434));
#4273=CARTESIAN_POINT('Ctrl Pts',(104.958734125,8.25000000136558,-43.4753311640868));
#4274=CARTESIAN_POINT('Ctrl Pts',(104.958734125,8.18750000136558,-1.28537377788739E-14));
#4275=CARTESIAN_POINT('Origin',(-7.105427357601E-14,49.5625000013656,-6.0924204042587E-14));
#4276=CARTESIAN_POINT('',(104.958734125,10.1875000013656,-6.0924204042587E-14));
#4277=CARTESIAN_POINT('',(104.958734125,9.93750000136558,-6.0924204042587E-14));
#4278=CARTESIAN_POINT('',(104.958734125,49.5625000013656,-1.089946703063E-13));
#4279=CARTESIAN_POINT('Ctrl Pts',(104.958734125,9.93750000136558,-1.28537377788739E-14));
#4280=CARTESIAN_POINT('Ctrl Pts',(104.958734125,9.87500000136558,43.4753311640868));
#4281=CARTESIAN_POINT('Ctrl Pts',(74.2170326445434,9.81250000136558,74.2170326445434));
#4282=CARTESIAN_POINT('Ctrl Pts',(43.4753311640869,9.75000000136558,104.958734125));
#4283=CARTESIAN_POINT('Ctrl Pts',(1.92806066683109E-14,9.68750000136558,
104.958734125));
#4284=CARTESIAN_POINT('Ctrl Pts',(-43.4753311640868,9.62500000136558,104.958734125));
#4285=CARTESIAN_POINT('Ctrl Pts',(-74.2170326445434,9.56250000136558,74.2170326445434));
#4286=CARTESIAN_POINT('Ctrl Pts',(-104.958734125,9.50000000136558,43.4753311640869));
#4287=CARTESIAN_POINT('Ctrl Pts',(-104.958734125,9.43750000136558,0.));
#4288=CARTESIAN_POINT('Ctrl Pts',(-104.958734125,9.37500000136558,-43.4753311640868));
#4289=CARTESIAN_POINT('Ctrl Pts',(-74.2170326445434,9.31250000136558,-74.2170326445434));
#4290=CARTESIAN_POINT('Ctrl Pts',(-43.4753311640868,9.25000000136558,-104.958734125));
#4291=CARTESIAN_POINT('Ctrl Pts',(-6.42686888943697E-15,9.18750000136558,
-104.958734125));
#4292=CARTESIAN_POINT('Ctrl Pts',(43.4753311640868,9.12500000136558,-104.958734125));
#4293=CARTESIAN_POINT('Ctrl Pts',(74.2170326445434,9.06250000136558,-74.2170326445434));
#4294=CARTESIAN_POINT('Ctrl Pts',(104.958734125,9.00000000136558,-43.4753311640868));
#4295=CARTESIAN_POINT('Ctrl Pts',(104.958734125,8.93750000136558,-1.28537377788739E-14));
#4296=CARTESIAN_POINT('Ctrl Pts',(104.958734125,10.1875000013656,-1.28537377788739E-14));
#4297=CARTESIAN_POINT('Ctrl Pts',(104.958734125,10.1250000013656,43.4753311640868));
#4298=CARTESIAN_POINT('Ctrl Pts',(74.2170326445434,10.0625000013656,74.2170326445434));
#4299=CARTESIAN_POINT('Ctrl Pts',(43.4753311640869,10.0000000013656,104.958734125));
#4300=CARTESIAN_POINT('Ctrl Pts',(1.92806066683109E-14,9.93750000136558,
104.958734125));
#4301=CARTESIAN_POINT('Ctrl Pts',(-43.4753311640868,9.87500000136558,104.958734125));
#4302=CARTESIAN_POINT('Ctrl Pts',(-74.2170326445434,9.81250000136558,74.2170326445434));
#4303=CARTESIAN_POINT('Ctrl Pts',(-104.958734125,9.75000000136558,43.4753311640869));
#4304=CARTESIAN_POINT('Ctrl Pts',(-104.958734125,9.68750000136558,0.));
#4305=CARTESIAN_POINT('Ctrl Pts',(-104.958734125,9.62500000136558,-43.4753311640868));
#4306=CARTESIAN_POINT('Ctrl Pts',(-74.2170326445434,9.56250000136558,-74.2170326445434));
#4307=CARTESIAN_POINT('Ctrl Pts',(-43.4753311640868,9.50000000136558,-104.958734125));
#4308=CARTESIAN_POINT('Ctrl Pts',(-6.42686888943697E-15,9.43750000136558,
-104.958734125));
#4309=CARTESIAN_POINT('Ctrl Pts',(43.4753311640868,9.37500000136558,-104.958734125));
#4310=CARTESIAN_POINT('Ctrl Pts',(74.2170326445434,9.31250000136558,-74.2170326445434));
#4311=CARTESIAN_POINT('Ctrl Pts',(104.958734125,9.25000000136558,-43.4753311640868));
#4312=CARTESIAN_POINT('Ctrl Pts',(104.958734125,9.18750000136558,-1.28537377788739E-14));
#4313=CARTESIAN_POINT('Origin',(-7.105427357601E-14,49.5625000013656,-6.0924204042587E-14));
#4314=CARTESIAN_POINT('',(104.958734125,11.1875000013656,-6.0924204042587E-14));
#4315=CARTESIAN_POINT('',(104.958734125,10.9375000013656,-6.0924204042587E-14));
#4316=CARTESIAN_POINT('',(104.958734125,49.5625000013656,-1.089946703063E-13));
#4317=CARTESIAN_POINT('Ctrl Pts',(104.958734125,10.9375000013656,-1.28537377788739E-14));
#4318=CARTESIAN_POINT('Ctrl Pts',(104.958734125,10.8750000013656,43.4753311640868));
#4319=CARTESIAN_POINT('Ctrl Pts',(74.2170326445434,10.8125000013656,74.2170326445434));
#4320=CARTESIAN_POINT('Ctrl Pts',(43.4753311640869,10.7500000013656,104.958734125));
#4321=CARTESIAN_POINT('Ctrl Pts',(1.92806066683109E-14,10.6875000013656,
104.958734125));
#4322=CARTESIAN_POINT('Ctrl Pts',(-43.4753311640868,10.6250000013656,104.958734125));
#4323=CARTESIAN_POINT('Ctrl Pts',(-74.2170326445434,10.5625000013656,74.2170326445434));
#4324=CARTESIAN_POINT('Ctrl Pts',(-104.958734125,10.5000000013656,43.4753311640869));
#4325=CARTESIAN_POINT('Ctrl Pts',(-104.958734125,10.4375000013656,0.));
#4326=CARTESIAN_POINT('Ctrl Pts',(-104.958734125,10.3750000013656,-43.4753311640868));
#4327=CARTESIAN_POINT('Ctrl Pts',(-74.2170326445434,10.3125000013656,-74.2170326445434));
#4328=CARTESIAN_POINT('Ctrl Pts',(-43.4753311640868,10.2500000013656,-104.958734125));
#4329=CARTESIAN_POINT('Ctrl Pts',(-6.42686888943697E-15,10.1875000013656,
-104.958734125));
#4330=CARTESIAN_POINT('Ctrl Pts',(43.4753311640868,10.1250000013656,-104.958734125));
#4331=CARTESIAN_POINT('Ctrl Pts',(74.2170326445434,10.0625000013656,-74.2170326445434));
#4332=CARTESIAN_POINT('Ctrl Pts',(104.958734125,10.0000000013656,-43.4753311640868));
#4333=CARTESIAN_POINT('Ctrl Pts',(104.958734125,9.93750000136558,-1.28537377788739E-14));
#4334=CARTESIAN_POINT('Ctrl Pts',(104.958734125,11.1875000013656,-1.28537377788739E-14));
#4335=CARTESIAN_POINT('Ctrl Pts',(104.958734125,11.1250000013656,43.4753311640868));
#4336=CARTESIAN_POINT('Ctrl Pts',(74.2170326445434,11.0625000013656,74.2170326445434));
#4337=CARTESIAN_POINT('Ctrl Pts',(43.4753311640869,11.0000000013656,104.958734125));
#4338=CARTESIAN_POINT('Ctrl Pts',(1.92806066683109E-14,10.9375000013656,
104.958734125));
#4339=CARTESIAN_POINT('Ctrl Pts',(-43.4753311640868,10.8750000013656,104.958734125));
#4340=CARTESIAN_POINT('Ctrl Pts',(-74.2170326445434,10.8125000013656,74.2170326445434));
#4341=CARTESIAN_POINT('Ctrl Pts',(-104.958734125,10.7500000013656,43.4753311640869));
#4342=CARTESIAN_POINT('Ctrl Pts',(-104.958734125,10.6875000013656,0.));
#4343=CARTESIAN_POINT('Ctrl Pts',(-104.958734125,10.6250000013656,-43.4753311640868));
#4344=CARTESIAN_POINT('Ctrl Pts',(-74.2170326445434,10.5625000013656,-74.2170326445434));
#4345=CARTESIAN_POINT('Ctrl Pts',(-43.4753311640868,10.5000000013656,-104.958734125));
#4346=CARTESIAN_POINT('Ctrl Pts',(-6.42686888943697E-15,10.4375000013656,
-104.958734125));
#4347=CARTESIAN_POINT('Ctrl Pts',(43.4753311640868,10.3750000013656,-104.958734125));
#4348=CARTESIAN_POINT('Ctrl Pts',(74.2170326445434,10.3125000013656,-74.2170326445434));
#4349=CARTESIAN_POINT('Ctrl Pts',(104.958734125,10.2500000013656,-43.4753311640868));
#4350=CARTESIAN_POINT('Ctrl Pts',(104.958734125,10.1875000013656,-1.28537377788739E-14));
#4351=CARTESIAN_POINT('Origin',(-7.105427357601E-14,49.5625000013656,-6.0924204042587E-14));
#4352=CARTESIAN_POINT('',(104.958734125,12.1875000013656,-6.0924204042587E-14));
#4353=CARTESIAN_POINT('',(104.958734125,11.9375000013656,-6.0924204042587E-14));
#4354=CARTESIAN_POINT('',(104.958734125,49.5625000013656,-1.089946703063E-13));
#4355=CARTESIAN_POINT('Ctrl Pts',(104.958734125,11.9375000013656,-1.28537377788739E-14));
#4356=CARTESIAN_POINT('Ctrl Pts',(104.958734125,11.8750000013656,43.4753311640868));
#4357=CARTESIAN_POINT('Ctrl Pts',(74.2170326445434,11.8125000013656,74.2170326445434));
#4358=CARTESIAN_POINT('Ctrl Pts',(43.4753311640869,11.7500000013656,104.958734125));
#4359=CARTESIAN_POINT('Ctrl Pts',(1.92806066683109E-14,11.6875000013656,
104.958734125));
#4360=CARTESIAN_POINT('Ctrl Pts',(-43.4753311640868,11.6250000013656,104.958734125));
#4361=CARTESIAN_POINT('Ctrl Pts',(-74.2170326445434,11.5625000013656,74.2170326445434));
#4362=CARTESIAN_POINT('Ctrl Pts',(-104.958734125,11.5000000013656,43.4753311640869));
#4363=CARTESIAN_POINT('Ctrl Pts',(-104.958734125,11.4375000013656,0.));
#4364=CARTESIAN_POINT('Ctrl Pts',(-104.958734125,11.3750000013656,-43.4753311640868));
#4365=CARTESIAN_POINT('Ctrl Pts',(-74.2170326445434,11.3125000013656,-74.2170326445434));
#4366=CARTESIAN_POINT('Ctrl Pts',(-43.4753311640868,11.2500000013656,-104.958734125));
#4367=CARTESIAN_POINT('Ctrl Pts',(-6.42686888943697E-15,11.1875000013656,
-104.958734125));
#4368=CARTESIAN_POINT('Ctrl Pts',(43.4753311640868,11.1250000013656,-104.958734125));
#4369=CARTESIAN_POINT('Ctrl Pts',(74.2170326445434,11.0625000013656,-74.2170326445434));
#4370=CARTESIAN_POINT('Ctrl Pts',(104.958734125,11.0000000013656,-43.4753311640868));
#4371=CARTESIAN_POINT('Ctrl Pts',(104.958734125,10.9375000013656,-1.28537377788739E-14));
#4372=CARTESIAN_POINT('Ctrl Pts',(104.958734125,12.1875000013656,-1.28537377788739E-14));
#4373=CARTESIAN_POINT('Ctrl Pts',(104.958734125,12.1250000013656,43.4753311640868));
#4374=CARTESIAN_POINT('Ctrl Pts',(74.2170326445434,12.0625000013656,74.2170326445434));
#4375=CARTESIAN_POINT('Ctrl Pts',(43.4753311640869,12.0000000013656,104.958734125));
#4376=CARTESIAN_POINT('Ctrl Pts',(1.92806066683109E-14,11.9375000013656,
104.958734125));
#4377=CARTESIAN_POINT('Ctrl Pts',(-43.4753311640868,11.8750000013656,104.958734125));
#4378=CARTESIAN_POINT('Ctrl Pts',(-74.2170326445434,11.8125000013656,74.2170326445434));
#4379=CARTESIAN_POINT('Ctrl Pts',(-104.958734125,11.7500000013656,43.4753311640869));
#4380=CARTESIAN_POINT('Ctrl Pts',(-104.958734125,11.6875000013656,0.));
#4381=CARTESIAN_POINT('Ctrl Pts',(-104.958734125,11.6250000013656,-43.4753311640868));
#4382=CARTESIAN_POINT('Ctrl Pts',(-74.2170326445434,11.5625000013656,-74.2170326445434));
#4383=CARTESIAN_POINT('Ctrl Pts',(-43.4753311640868,11.5000000013656,-104.958734125));
#4384=CARTESIAN_POINT('Ctrl Pts',(-6.42686888943697E-15,11.4375000013656,
-104.958734125));
#4385=CARTESIAN_POINT('Ctrl Pts',(43.4753311640868,11.3750000013656,-104.958734125));
#4386=CARTESIAN_POINT('Ctrl Pts',(74.2170326445434,11.3125000013656,-74.2170326445434));
#4387=CARTESIAN_POINT('Ctrl Pts',(104.958734125,11.2500000013656,-43.4753311640868));
#4388=CARTESIAN_POINT('Ctrl Pts',(104.958734125,11.1875000013656,-1.28537377788739E-14));
#4389=CARTESIAN_POINT('Origin',(-7.105427357601E-14,49.5625000013656,-6.0924204042587E-14));
#4390=CARTESIAN_POINT('',(104.958734125,13.1875000013656,-6.0924204042587E-14));
#4391=CARTESIAN_POINT('',(104.958734125,12.9375000013656,-6.0924204042587E-14));
#4392=CARTESIAN_POINT('',(104.958734125,49.5625000013656,-1.089946703063E-13));
#4393=CARTESIAN_POINT('Ctrl Pts',(104.958734125,12.9375000013656,-1.28537377788739E-14));
#4394=CARTESIAN_POINT('Ctrl Pts',(104.958734125,12.8750000013656,43.4753311640868));
#4395=CARTESIAN_POINT('Ctrl Pts',(74.2170326445434,12.8125000013656,74.2170326445434));
#4396=CARTESIAN_POINT('Ctrl Pts',(43.4753311640869,12.7500000013656,104.958734125));
#4397=CARTESIAN_POINT('Ctrl Pts',(1.92806066683109E-14,12.6875000013656,
104.958734125));
#4398=CARTESIAN_POINT('Ctrl Pts',(-43.4753311640868,12.6250000013656,104.958734125));
#4399=CARTESIAN_POINT('Ctrl Pts',(-74.2170326445434,12.5625000013656,74.2170326445434));
#4400=CARTESIAN_POINT('Ctrl Pts',(-104.958734125,12.5000000013656,43.4753311640869));
#4401=CARTESIAN_POINT('Ctrl Pts',(-104.958734125,12.4375000013656,0.));
#4402=CARTESIAN_POINT('Ctrl Pts',(-104.958734125,12.3750000013656,-43.4753311640868));
#4403=CARTESIAN_POINT('Ctrl Pts',(-74.2170326445434,12.3125000013656,-74.2170326445434));
#4404=CARTESIAN_POINT('Ctrl Pts',(-43.4753311640868,12.2500000013656,-104.958734125));
#4405=CARTESIAN_POINT('Ctrl Pts',(-6.42686888943697E-15,12.1875000013656,
-104.958734125));
#4406=CARTESIAN_POINT('Ctrl Pts',(43.4753311640868,12.1250000013656,-104.958734125));
#4407=CARTESIAN_POINT('Ctrl Pts',(74.2170326445434,12.0625000013656,-74.2170326445434));
#4408=CARTESIAN_POINT('Ctrl Pts',(104.958734125,12.0000000013656,-43.4753311640868));
#4409=CARTESIAN_POINT('Ctrl Pts',(104.958734125,11.9375000013656,-1.28537377788739E-14));
#4410=CARTESIAN_POINT('Ctrl Pts',(104.958734125,13.1875000013656,-1.28537377788739E-14));
#4411=CARTESIAN_POINT('Ctrl Pts',(104.958734125,13.1250000013656,43.4753311640868));
#4412=CARTESIAN_POINT('Ctrl Pts',(74.2170326445434,13.0625000013656,74.2170326445434));
#4413=CARTESIAN_POINT('Ctrl Pts',(43.4753311640869,13.0000000013656,104.958734125));
#4414=CARTESIAN_POINT('Ctrl Pts',(1.92806066683109E-14,12.9375000013656,
104.958734125));
#4415=CARTESIAN_POINT('Ctrl Pts',(-43.4753311640868,12.8750000013656,104.958734125));
#4416=CARTESIAN_POINT('Ctrl Pts',(-74.2170326445434,12.8125000013656,74.2170326445434));
#4417=CARTESIAN_POINT('Ctrl Pts',(-104.958734125,12.7500000013656,43.4753311640869));
#4418=CARTESIAN_POINT('Ctrl Pts',(-104.958734125,12.6875000013656,0.));
#4419=CARTESIAN_POINT('Ctrl Pts',(-104.958734125,12.6250000013656,-43.4753311640868));
#4420=CARTESIAN_POINT('Ctrl Pts',(-74.2170326445434,12.5625000013656,-74.2170326445434));
#4421=CARTESIAN_POINT('Ctrl Pts',(-43.4753311640868,12.5000000013656,-104.958734125));
#4422=CARTESIAN_POINT('Ctrl Pts',(-6.42686888943697E-15,12.4375000013656,
-104.958734125));
#4423=CARTESIAN_POINT('Ctrl Pts',(43.4753311640868,12.3750000013656,-104.958734125));
#4424=CARTESIAN_POINT('Ctrl Pts',(74.2170326445434,12.3125000013656,-74.2170326445434));
#4425=CARTESIAN_POINT('Ctrl Pts',(104.958734125,12.2500000013656,-43.4753311640868));
#4426=CARTESIAN_POINT('Ctrl Pts',(104.958734125,12.1875000013656,-1.28537377788739E-14));
#4427=CARTESIAN_POINT('Origin',(-7.105427357601E-14,49.5625000013656,-6.0924204042587E-14));
#4428=CARTESIAN_POINT('',(104.958734125,14.1875000013656,-6.0924204042587E-14));
#4429=CARTESIAN_POINT('',(104.958734125,13.9375000013656,-6.0924204042587E-14));
#4430=CARTESIAN_POINT('',(104.958734125,49.5625000013656,-1.089946703063E-13));
#4431=CARTESIAN_POINT('Ctrl Pts',(104.958734125,13.9375000013656,-1.28537377788739E-14));
#4432=CARTESIAN_POINT('Ctrl Pts',(104.958734125,13.8750000013656,43.4753311640868));
#4433=CARTESIAN_POINT('Ctrl Pts',(74.2170326445434,13.8125000013656,74.2170326445434));
#4434=CARTESIAN_POINT('Ctrl Pts',(43.4753311640869,13.7500000013656,104.958734125));
#4435=CARTESIAN_POINT('Ctrl Pts',(1.92806066683109E-14,13.6875000013656,
104.958734125));
#4436=CARTESIAN_POINT('Ctrl Pts',(-43.4753311640868,13.6250000013656,104.958734125));
#4437=CARTESIAN_POINT('Ctrl Pts',(-74.2170326445434,13.5625000013656,74.2170326445434));
#4438=CARTESIAN_POINT('Ctrl Pts',(-104.958734125,13.5000000013656,43.4753311640869));
#4439=CARTESIAN_POINT('Ctrl Pts',(-104.958734125,13.4375000013656,0.));
#4440=CARTESIAN_POINT('Ctrl Pts',(-104.958734125,13.3750000013656,-43.4753311640868));
#4441=CARTESIAN_POINT('Ctrl Pts',(-74.2170326445434,13.3125000013656,-74.2170326445434));
#4442=CARTESIAN_POINT('Ctrl Pts',(-43.4753311640868,13.2500000013656,-104.958734125));
#4443=CARTESIAN_POINT('Ctrl Pts',(-6.42686888943697E-15,13.1875000013656,
-104.958734125));
#4444=CARTESIAN_POINT('Ctrl Pts',(43.4753311640868,13.1250000013656,-104.958734125));
#4445=CARTESIAN_POINT('Ctrl Pts',(74.2170326445434,13.0625000013656,-74.2170326445434));
#4446=CARTESIAN_POINT('Ctrl Pts',(104.958734125,13.0000000013656,-43.4753311640868));
#4447=CARTESIAN_POINT('Ctrl Pts',(104.958734125,12.9375000013656,-1.28537377788739E-14));
#4448=CARTESIAN_POINT('Ctrl Pts',(104.958734125,14.1875000013656,-1.28537377788739E-14));
#4449=CARTESIAN_POINT('Ctrl Pts',(104.958734125,14.1250000013656,43.4753311640868));
#4450=CARTESIAN_POINT('Ctrl Pts',(74.2170326445434,14.0625000013656,74.2170326445434));
#4451=CARTESIAN_POINT('Ctrl Pts',(43.4753311640869,14.0000000013656,104.958734125));
#4452=CARTESIAN_POINT('Ctrl Pts',(1.92806066683109E-14,13.9375000013656,
104.958734125));
#4453=CARTESIAN_POINT('Ctrl Pts',(-43.4753311640868,13.8750000013656,104.958734125));
#4454=CARTESIAN_POINT('Ctrl Pts',(-74.2170326445434,13.8125000013656,74.2170326445434));
#4455=CARTESIAN_POINT('Ctrl Pts',(-104.958734125,13.7500000013656,43.4753311640869));
#4456=CARTESIAN_POINT('Ctrl Pts',(-104.958734125,13.6875000013656,0.));
#4457=CARTESIAN_POINT('Ctrl Pts',(-104.958734125,13.6250000013656,-43.4753311640868));
#4458=CARTESIAN_POINT('Ctrl Pts',(-74.2170326445434,13.5625000013656,-74.2170326445434));
#4459=CARTESIAN_POINT('Ctrl Pts',(-43.4753311640868,13.5000000013656,-104.958734125));
#4460=CARTESIAN_POINT('Ctrl Pts',(-6.42686888943697E-15,13.4375000013656,
-104.958734125));
#4461=CARTESIAN_POINT('Ctrl Pts',(43.4753311640868,13.3750000013656,-104.958734125));
#4462=CARTESIAN_POINT('Ctrl Pts',(74.2170326445434,13.3125000013656,-74.2170326445434));
#4463=CARTESIAN_POINT('Ctrl Pts',(104.958734125,13.2500000013656,-43.4753311640868));
#4464=CARTESIAN_POINT('Ctrl Pts',(104.958734125,13.1875000013656,-1.28537377788739E-14));
#4465=CARTESIAN_POINT('Origin',(-7.105427357601E-14,49.5625000013656,-6.0924204042587E-14));
#4466=CARTESIAN_POINT('',(104.958734125,15.1875000013656,-6.0924204042587E-14));
#4467=CARTESIAN_POINT('',(104.958734125,14.9375000013656,-6.0924204042587E-14));
#4468=CARTESIAN_POINT('',(104.958734125,49.5625000013656,-1.089946703063E-13));
#4469=CARTESIAN_POINT('Ctrl Pts',(104.958734125,14.9375000013656,-1.28537377788739E-14));
#4470=CARTESIAN_POINT('Ctrl Pts',(104.958734125,14.8750000013656,43.4753311640868));
#4471=CARTESIAN_POINT('Ctrl Pts',(74.2170326445434,14.8125000013656,74.2170326445434));
#4472=CARTESIAN_POINT('Ctrl Pts',(43.4753311640869,14.7500000013656,104.958734125));
#4473=CARTESIAN_POINT('Ctrl Pts',(1.92806066683109E-14,14.6875000013656,
104.958734125));
#4474=CARTESIAN_POINT('Ctrl Pts',(-43.4753311640868,14.6250000013656,104.958734125));
#4475=CARTESIAN_POINT('Ctrl Pts',(-74.2170326445434,14.5625000013656,74.2170326445434));
#4476=CARTESIAN_POINT('Ctrl Pts',(-104.958734125,14.5000000013656,43.4753311640869));
#4477=CARTESIAN_POINT('Ctrl Pts',(-104.958734125,14.4375000013656,0.));
#4478=CARTESIAN_POINT('Ctrl Pts',(-104.958734125,14.3750000013656,-43.4753311640868));
#4479=CARTESIAN_POINT('Ctrl Pts',(-74.2170326445434,14.3125000013656,-74.2170326445434));
#4480=CARTESIAN_POINT('Ctrl Pts',(-43.4753311640868,14.2500000013656,-104.958734125));
#4481=CARTESIAN_POINT('Ctrl Pts',(-6.42686888943697E-15,14.1875000013656,
-104.958734125));
#4482=CARTESIAN_POINT('Ctrl Pts',(43.4753311640868,14.1250000013656,-104.958734125));
#4483=CARTESIAN_POINT('Ctrl Pts',(74.2170326445434,14.0625000013656,-74.2170326445434));
#4484=CARTESIAN_POINT('Ctrl Pts',(104.958734125,14.0000000013656,-43.4753311640868));
#4485=CARTESIAN_POINT('Ctrl Pts',(104.958734125,13.9375000013656,-1.28537377788739E-14));
#4486=CARTESIAN_POINT('Ctrl Pts',(104.958734125,15.1875000013656,-1.28537377788739E-14));
#4487=CARTESIAN_POINT('Ctrl Pts',(104.958734125,15.1250000013656,43.4753311640868));
#4488=CARTESIAN_POINT('Ctrl Pts',(74.2170326445434,15.0625000013656,74.2170326445434));
#4489=CARTESIAN_POINT('Ctrl Pts',(43.4753311640869,15.0000000013656,104.958734125));
#4490=CARTESIAN_POINT('Ctrl Pts',(1.92806066683109E-14,14.9375000013656,
104.958734125));
#4491=CARTESIAN_POINT('Ctrl Pts',(-43.4753311640868,14.8750000013656,104.958734125));
#4492=CARTESIAN_POINT('Ctrl Pts',(-74.2170326445434,14.8125000013656,74.2170326445434));
#4493=CARTESIAN_POINT('Ctrl Pts',(-104.958734125,14.7500000013656,43.4753311640869));
#4494=CARTESIAN_POINT('Ctrl Pts',(-104.958734125,14.6875000013656,0.));
#4495=CARTESIAN_POINT('Ctrl Pts',(-104.958734125,14.6250000013656,-43.4753311640868));
#4496=CARTESIAN_POINT('Ctrl Pts',(-74.2170326445434,14.5625000013656,-74.2170326445434));
#4497=CARTESIAN_POINT('Ctrl Pts',(-43.4753311640868,14.5000000013656,-104.958734125));
#4498=CARTESIAN_POINT('Ctrl Pts',(-6.42686888943697E-15,14.4375000013656,
-104.958734125));
#4499=CARTESIAN_POINT('Ctrl Pts',(43.4753311640868,14.3750000013656,-104.958734125));
#4500=CARTESIAN_POINT('Ctrl Pts',(74.2170326445434,14.3125000013656,-74.2170326445434));
#4501=CARTESIAN_POINT('Ctrl Pts',(104.958734125,14.2500000013656,-43.4753311640868));
#4502=CARTESIAN_POINT('Ctrl Pts',(104.958734125,14.1875000013656,-1.28537377788739E-14));
#4503=CARTESIAN_POINT('Origin',(-7.105427357601E-14,49.5625000013656,-6.0924204042587E-14));
#4504=CARTESIAN_POINT('',(104.958734125,16.1875000013656,-6.0924204042587E-14));
#4505=CARTESIAN_POINT('',(104.958734125,15.9375000013656,-6.0924204042587E-14));
#4506=CARTESIAN_POINT('',(104.958734125,49.5625000013656,-1.089946703063E-13));
#4507=CARTESIAN_POINT('Ctrl Pts',(104.958734125,15.9375000013656,-1.28537377788739E-14));
#4508=CARTESIAN_POINT('Ctrl Pts',(104.958734125,15.8750000013656,43.4753311640868));
#4509=CARTESIAN_POINT('Ctrl Pts',(74.2170326445434,15.8125000013656,74.2170326445434));
#4510=CARTESIAN_POINT('Ctrl Pts',(43.4753311640869,15.7500000013656,104.958734125));
#4511=CARTESIAN_POINT('Ctrl Pts',(1.92806066683109E-14,15.6875000013656,
104.958734125));
#4512=CARTESIAN_POINT('Ctrl Pts',(-43.4753311640868,15.6250000013656,104.958734125));
#4513=CARTESIAN_POINT('Ctrl Pts',(-74.2170326445434,15.5625000013656,74.2170326445434));
#4514=CARTESIAN_POINT('Ctrl Pts',(-104.958734125,15.5000000013656,43.4753311640869));
#4515=CARTESIAN_POINT('Ctrl Pts',(-104.958734125,15.4375000013656,0.));
#4516=CARTESIAN_POINT('Ctrl Pts',(-104.958734125,15.3750000013656,-43.4753311640868));
#4517=CARTESIAN_POINT('Ctrl Pts',(-74.2170326445434,15.3125000013656,-74.2170326445434));
#4518=CARTESIAN_POINT('Ctrl Pts',(-43.4753311640868,15.2500000013656,-104.958734125));
#4519=CARTESIAN_POINT('Ctrl Pts',(-6.42686888943697E-15,15.1875000013656,
-104.958734125));
#4520=CARTESIAN_POINT('Ctrl Pts',(43.4753311640868,15.1250000013656,-104.958734125));
#4521=CARTESIAN_POINT('Ctrl Pts',(74.2170326445434,15.0625000013656,-74.2170326445434));
#4522=CARTESIAN_POINT('Ctrl Pts',(104.958734125,15.0000000013656,-43.4753311640868));
#4523=CARTESIAN_POINT('Ctrl Pts',(104.958734125,14.9375000013656,-1.28537377788739E-14));
#4524=CARTESIAN_POINT('Ctrl Pts',(104.958734125,16.1875000013656,-1.28537377788739E-14));
#4525=CARTESIAN_POINT('Ctrl Pts',(104.958734125,16.1250000013656,43.4753311640868));
#4526=CARTESIAN_POINT('Ctrl Pts',(74.2170326445434,16.0625000013656,74.2170326445434));
#4527=CARTESIAN_POINT('Ctrl Pts',(43.4753311640869,16.0000000013656,104.958734125));
#4528=CARTESIAN_POINT('Ctrl Pts',(1.92806066683109E-14,15.9375000013656,
104.958734125));
#4529=CARTESIAN_POINT('Ctrl Pts',(-43.4753311640868,15.8750000013656,104.958734125));
#4530=CARTESIAN_POINT('Ctrl Pts',(-74.2170326445434,15.8125000013656,74.2170326445434));
#4531=CARTESIAN_POINT('Ctrl Pts',(-104.958734125,15.7500000013656,43.4753311640869));
#4532=CARTESIAN_POINT('Ctrl Pts',(-104.958734125,15.6875000013656,0.));
#4533=CARTESIAN_POINT('Ctrl Pts',(-104.958734125,15.6250000013656,-43.4753311640868));
#4534=CARTESIAN_POINT('Ctrl Pts',(-74.2170326445434,15.5625000013656,-74.2170326445434));
#4535=CARTESIAN_POINT('Ctrl Pts',(-43.4753311640868,15.5000000013656,-104.958734125));
#4536=CARTESIAN_POINT('Ctrl Pts',(-6.42686888943697E-15,15.4375000013656,
-104.958734125));
#4537=CARTESIAN_POINT('Ctrl Pts',(43.4753311640868,15.3750000013656,-104.958734125));
#4538=CARTESIAN_POINT('Ctrl Pts',(74.2170326445434,15.3125000013656,-74.2170326445434));
#4539=CARTESIAN_POINT('Ctrl Pts',(104.958734125,15.2500000013656,-43.4753311640868));
#4540=CARTESIAN_POINT('Ctrl Pts',(104.958734125,15.1875000013656,-1.28537377788739E-14));
#4541=CARTESIAN_POINT('Origin',(-7.105427357601E-14,49.5625000013656,-6.0924204042587E-14));
#4542=CARTESIAN_POINT('',(104.958734125,17.1875000013656,-6.0924204042587E-14));
#4543=CARTESIAN_POINT('',(104.958734125,16.9375000013656,-6.0924204042587E-14));
#4544=CARTESIAN_POINT('',(104.958734125,49.5625000013656,-1.089946703063E-13));
#4545=CARTESIAN_POINT('Ctrl Pts',(104.958734125,16.9375000013656,-1.28537377788739E-14));
#4546=CARTESIAN_POINT('Ctrl Pts',(104.958734125,16.8750000013656,43.4753311640868));
#4547=CARTESIAN_POINT('Ctrl Pts',(74.2170326445434,16.8125000013656,74.2170326445434));
#4548=CARTESIAN_POINT('Ctrl Pts',(43.4753311640869,16.7500000013656,104.958734125));
#4549=CARTESIAN_POINT('Ctrl Pts',(1.92806066683109E-14,16.6875000013656,
104.958734125));
#4550=CARTESIAN_POINT('Ctrl Pts',(-43.4753311640868,16.6250000013656,104.958734125));
#4551=CARTESIAN_POINT('Ctrl Pts',(-74.2170326445434,16.5625000013656,74.2170326445434));
#4552=CARTESIAN_POINT('Ctrl Pts',(-104.958734125,16.5000000013656,43.4753311640869));
#4553=CARTESIAN_POINT('Ctrl Pts',(-104.958734125,16.4375000013656,0.));
#4554=CARTESIAN_POINT('Ctrl Pts',(-104.958734125,16.3750000013656,-43.4753311640868));
#4555=CARTESIAN_POINT('Ctrl Pts',(-74.2170326445434,16.3125000013656,-74.2170326445434));
#4556=CARTESIAN_POINT('Ctrl Pts',(-43.4753311640868,16.2500000013656,-104.958734125));
#4557=CARTESIAN_POINT('Ctrl Pts',(-6.42686888943697E-15,16.1875000013656,
-104.958734125));
#4558=CARTESIAN_POINT('Ctrl Pts',(43.4753311640868,16.1250000013656,-104.958734125));
#4559=CARTESIAN_POINT('Ctrl Pts',(74.2170326445434,16.0625000013656,-74.2170326445434));
#4560=CARTESIAN_POINT('Ctrl Pts',(104.958734125,16.0000000013656,-43.4753311640868));
#4561=CARTESIAN_POINT('Ctrl Pts',(104.958734125,15.9375000013656,-1.28537377788739E-14));
#4562=CARTESIAN_POINT('Ctrl Pts',(104.958734125,17.1875000013656,-1.28537377788739E-14));
#4563=CARTESIAN_POINT('Ctrl Pts',(104.958734125,17.1250000013656,43.4753311640868));
#4564=CARTESIAN_POINT('Ctrl Pts',(74.2170326445434,17.0625000013656,74.2170326445434));
#4565=CARTESIAN_POINT('Ctrl Pts',(43.4753311640869,17.0000000013656,104.958734125));
#4566=CARTESIAN_POINT('Ctrl Pts',(1.92806066683109E-14,16.9375000013656,
104.958734125));
#4567=CARTESIAN_POINT('Ctrl Pts',(-43.4753311640868,16.8750000013656,104.958734125));
#4568=CARTESIAN_POINT('Ctrl Pts',(-74.2170326445434,16.8125000013656,74.2170326445434));
#4569=CARTESIAN_POINT('Ctrl Pts',(-104.958734125,16.7500000013656,43.4753311640869));
#4570=CARTESIAN_POINT('Ctrl Pts',(-104.958734125,16.6875000013656,0.));
#4571=CARTESIAN_POINT('Ctrl Pts',(-104.958734125,16.6250000013656,-43.4753311640868));
#4572=CARTESIAN_POINT('Ctrl Pts',(-74.2170326445434,16.5625000013656,-74.2170326445434));
#4573=CARTESIAN_POINT('Ctrl Pts',(-43.4753311640868,16.5000000013656,-104.958734125));
#4574=CARTESIAN_POINT('Ctrl Pts',(-6.42686888943697E-15,16.4375000013656,
-104.958734125));
#4575=CARTESIAN_POINT('Ctrl Pts',(43.4753311640868,16.3750000013656,-104.958734125));
#4576=CARTESIAN_POINT('Ctrl Pts',(74.2170326445434,16.3125000013656,-74.2170326445434));
#4577=CARTESIAN_POINT('Ctrl Pts',(104.958734125,16.2500000013656,-43.4753311640868));
#4578=CARTESIAN_POINT('Ctrl Pts',(104.958734125,16.1875000013656,-1.28537377788739E-14));
#4579=CARTESIAN_POINT('Origin',(-7.105427357601E-14,49.5625000013656,-6.0924204042587E-14));
#4580=CARTESIAN_POINT('',(104.958734125,18.1875000013656,-6.0924204042587E-14));
#4581=CARTESIAN_POINT('',(104.958734125,17.9375000013656,-6.0924204042587E-14));
#4582=CARTESIAN_POINT('',(104.958734125,49.5625000013656,-1.089946703063E-13));
#4583=CARTESIAN_POINT('Ctrl Pts',(104.958734125,17.9375000013656,-1.28537377788739E-14));
#4584=CARTESIAN_POINT('Ctrl Pts',(104.958734125,17.8750000013656,43.4753311640868));
#4585=CARTESIAN_POINT('Ctrl Pts',(74.2170326445434,17.8125000013656,74.2170326445434));
#4586=CARTESIAN_POINT('Ctrl Pts',(43.4753311640869,17.7500000013656,104.958734125));
#4587=CARTESIAN_POINT('Ctrl Pts',(1.92806066683109E-14,17.6875000013656,
104.958734125));
#4588=CARTESIAN_POINT('Ctrl Pts',(-43.4753311640868,17.6250000013656,104.958734125));
#4589=CARTESIAN_POINT('Ctrl Pts',(-74.2170326445434,17.5625000013656,74.2170326445434));
#4590=CARTESIAN_POINT('Ctrl Pts',(-104.958734125,17.5000000013656,43.4753311640869));
#4591=CARTESIAN_POINT('Ctrl Pts',(-104.958734125,17.4375000013656,0.));
#4592=CARTESIAN_POINT('Ctrl Pts',(-104.958734125,17.3750000013656,-43.4753311640868));
#4593=CARTESIAN_POINT('Ctrl Pts',(-74.2170326445434,17.3125000013656,-74.2170326445434));
#4594=CARTESIAN_POINT('Ctrl Pts',(-43.4753311640868,17.2500000013656,-104.958734125));
#4595=CARTESIAN_POINT('Ctrl Pts',(-6.42686888943697E-15,17.1875000013656,
-104.958734125));
#4596=CARTESIAN_POINT('Ctrl Pts',(43.4753311640868,17.1250000013656,-104.958734125));
#4597=CARTESIAN_POINT('Ctrl Pts',(74.2170326445434,17.0625000013656,-74.2170326445434));
#4598=CARTESIAN_POINT('Ctrl Pts',(104.958734125,17.0000000013656,-43.4753311640868));
#4599=CARTESIAN_POINT('Ctrl Pts',(104.958734125,16.9375000013656,-1.28537377788739E-14));
#4600=CARTESIAN_POINT('Ctrl Pts',(104.958734125,18.1875000013656,-1.28537377788739E-14));
#4601=CARTESIAN_POINT('Ctrl Pts',(104.958734125,18.1250000013656,43.4753311640868));
#4602=CARTESIAN_POINT('Ctrl Pts',(74.2170326445434,18.0625000013656,74.2170326445434));
#4603=CARTESIAN_POINT('Ctrl Pts',(43.4753311640869,18.0000000013656,104.958734125));
#4604=CARTESIAN_POINT('Ctrl Pts',(1.92806066683109E-14,17.9375000013656,
104.958734125));
#4605=CARTESIAN_POINT('Ctrl Pts',(-43.4753311640868,17.8750000013656,104.958734125));
#4606=CARTESIAN_POINT('Ctrl Pts',(-74.2170326445434,17.8125000013656,74.2170326445434));
#4607=CARTESIAN_POINT('Ctrl Pts',(-104.958734125,17.7500000013656,43.4753311640869));
#4608=CARTESIAN_POINT('Ctrl Pts',(-104.958734125,17.6875000013656,0.));
#4609=CARTESIAN_POINT('Ctrl Pts',(-104.958734125,17.6250000013656,-43.4753311640868));
#4610=CARTESIAN_POINT('Ctrl Pts',(-74.2170326445434,17.5625000013656,-74.2170326445434));
#4611=CARTESIAN_POINT('Ctrl Pts',(-43.4753311640868,17.5000000013656,-104.958734125));
#4612=CARTESIAN_POINT('Ctrl Pts',(-6.42686888943697E-15,17.4375000013656,
-104.958734125));
#4613=CARTESIAN_POINT('Ctrl Pts',(43.4753311640868,17.3750000013656,-104.958734125));
#4614=CARTESIAN_POINT('Ctrl Pts',(74.2170326445434,17.3125000013656,-74.2170326445434));
#4615=CARTESIAN_POINT('Ctrl Pts',(104.958734125,17.2500000013656,-43.4753311640868));
#4616=CARTESIAN_POINT('Ctrl Pts',(104.958734125,17.1875000013656,-1.28537377788739E-14));
#4617=CARTESIAN_POINT('Origin',(-7.105427357601E-14,49.5625000013656,-6.0924204042587E-14));
#4618=CARTESIAN_POINT('',(104.958734125,19.1875000013656,-6.0924204042587E-14));
#4619=CARTESIAN_POINT('',(104.958734125,18.9375000013656,-6.0924204042587E-14));
#4620=CARTESIAN_POINT('',(104.958734125,49.5625000013656,-1.089946703063E-13));
#4621=CARTESIAN_POINT('Ctrl Pts',(104.958734125,18.9375000013656,-1.28537377788739E-14));
#4622=CARTESIAN_POINT('Ctrl Pts',(104.958734125,18.8750000013656,43.4753311640868));
#4623=CARTESIAN_POINT('Ctrl Pts',(74.2170326445434,18.8125000013656,74.2170326445434));
#4624=CARTESIAN_POINT('Ctrl Pts',(43.4753311640869,18.7500000013656,104.958734125));
#4625=CARTESIAN_POINT('Ctrl Pts',(1.92806066683109E-14,18.6875000013656,
104.958734125));
#4626=CARTESIAN_POINT('Ctrl Pts',(-43.4753311640868,18.6250000013656,104.958734125));
#4627=CARTESIAN_POINT('Ctrl Pts',(-74.2170326445434,18.5625000013656,74.2170326445434));
#4628=CARTESIAN_POINT('Ctrl Pts',(-104.958734125,18.5000000013656,43.4753311640869));
#4629=CARTESIAN_POINT('Ctrl Pts',(-104.958734125,18.4375000013656,0.));
#4630=CARTESIAN_POINT('Ctrl Pts',(-104.958734125,18.3750000013656,-43.4753311640868));
#4631=CARTESIAN_POINT('Ctrl Pts',(-74.2170326445434,18.3125000013656,-74.2170326445434));
#4632=CARTESIAN_POINT('Ctrl Pts',(-43.4753311640868,18.2500000013656,-104.958734125));
#4633=CARTESIAN_POINT('Ctrl Pts',(-6.42686888943697E-15,18.1875000013656,
-104.958734125));
#4634=CARTESIAN_POINT('Ctrl Pts',(43.4753311640868,18.1250000013656,-104.958734125));
#4635=CARTESIAN_POINT('Ctrl Pts',(74.2170326445434,18.0625000013656,-74.2170326445434));
#4636=CARTESIAN_POINT('Ctrl Pts',(104.958734125,18.0000000013656,-43.4753311640868));
#4637=CARTESIAN_POINT('Ctrl Pts',(104.958734125,17.9375000013656,-1.28537377788739E-14));
#4638=CARTESIAN_POINT('Ctrl Pts',(104.958734125,19.1875000013656,-1.28537377788739E-14));
#4639=CARTESIAN_POINT('Ctrl Pts',(104.958734125,19.1250000013656,43.4753311640868));
#4640=CARTESIAN_POINT('Ctrl Pts',(74.2170326445434,19.0625000013656,74.2170326445434));
#4641=CARTESIAN_POINT('Ctrl Pts',(43.4753311640869,19.0000000013656,104.958734125));
#4642=CARTESIAN_POINT('Ctrl Pts',(1.92806066683109E-14,18.9375000013656,
104.958734125));
#4643=CARTESIAN_POINT('Ctrl Pts',(-43.4753311640868,18.8750000013656,104.958734125));
#4644=CARTESIAN_POINT('Ctrl Pts',(-74.2170326445434,18.8125000013656,74.2170326445434));
#4645=CARTESIAN_POINT('Ctrl Pts',(-104.958734125,18.7500000013656,43.4753311640869));
#4646=CARTESIAN_POINT('Ctrl Pts',(-104.958734125,18.6875000013656,0.));
#4647=CARTESIAN_POINT('Ctrl Pts',(-104.958734125,18.6250000013656,-43.4753311640868));
#4648=CARTESIAN_POINT('Ctrl Pts',(-74.2170326445434,18.5625000013656,-74.2170326445434));
#4649=CARTESIAN_POINT('Ctrl Pts',(-43.4753311640868,18.5000000013656,-104.958734125));
#4650=CARTESIAN_POINT('Ctrl Pts',(-6.42686888943697E-15,18.4375000013656,
-104.958734125));
#4651=CARTESIAN_POINT('Ctrl Pts',(43.4753311640868,18.3750000013656,-104.958734125));
#4652=CARTESIAN_POINT('Ctrl Pts',(74.2170326445434,18.3125000013656,-74.2170326445434));
#4653=CARTESIAN_POINT('Ctrl Pts',(104.958734125,18.2500000013656,-43.4753311640868));
#4654=CARTESIAN_POINT('Ctrl Pts',(104.958734125,18.1875000013656,-1.28537377788739E-14));
#4655=CARTESIAN_POINT('Origin',(-7.105427357601E-14,49.5625000013656,-6.0924204042587E-14));
#4656=CARTESIAN_POINT('',(104.958734125,20.1875000013656,-6.0924204042587E-14));
#4657=CARTESIAN_POINT('',(104.958734125,19.9375000013656,-6.0924204042587E-14));
#4658=CARTESIAN_POINT('',(104.958734125,49.5625000013656,-1.089946703063E-13));
#4659=CARTESIAN_POINT('Ctrl Pts',(104.958734125,19.9375000013656,-1.28537377788739E-14));
#4660=CARTESIAN_POINT('Ctrl Pts',(104.958734125,19.8750000013656,43.4753311640868));
#4661=CARTESIAN_POINT('Ctrl Pts',(74.2170326445434,19.8125000013656,74.2170326445434));
#4662=CARTESIAN_POINT('Ctrl Pts',(43.4753311640869,19.7500000013656,104.958734125));
#4663=CARTESIAN_POINT('Ctrl Pts',(1.92806066683109E-14,19.6875000013656,
104.958734125));
#4664=CARTESIAN_POINT('Ctrl Pts',(-43.4753311640868,19.6250000013656,104.958734125));
#4665=CARTESIAN_POINT('Ctrl Pts',(-74.2170326445434,19.5625000013656,74.2170326445434));
#4666=CARTESIAN_POINT('Ctrl Pts',(-104.958734125,19.5000000013656,43.4753311640869));
#4667=CARTESIAN_POINT('Ctrl Pts',(-104.958734125,19.4375000013656,0.));
#4668=CARTESIAN_POINT('Ctrl Pts',(-104.958734125,19.3750000013656,-43.4753311640868));
#4669=CARTESIAN_POINT('Ctrl Pts',(-74.2170326445434,19.3125000013656,-74.2170326445434));
#4670=CARTESIAN_POINT('Ctrl Pts',(-43.4753311640868,19.2500000013656,-104.958734125));
#4671=CARTESIAN_POINT('Ctrl Pts',(-6.42686888943697E-15,19.1875000013656,
-104.958734125));
#4672=CARTESIAN_POINT('Ctrl Pts',(43.4753311640868,19.1250000013656,-104.958734125));
#4673=CARTESIAN_POINT('Ctrl Pts',(74.2170326445434,19.0625000013656,-74.2170326445434));
#4674=CARTESIAN_POINT('Ctrl Pts',(104.958734125,19.0000000013656,-43.4753311640868));
#4675=CARTESIAN_POINT('Ctrl Pts',(104.958734125,18.9375000013656,-1.28537377788739E-14));
#4676=CARTESIAN_POINT('Ctrl Pts',(104.958734125,20.1875000013656,-1.28537377788739E-14));
#4677=CARTESIAN_POINT('Ctrl Pts',(104.958734125,20.1250000013656,43.4753311640868));
#4678=CARTESIAN_POINT('Ctrl Pts',(74.2170326445434,20.0625000013656,74.2170326445434));
#4679=CARTESIAN_POINT('Ctrl Pts',(43.4753311640869,20.0000000013656,104.958734125));
#4680=CARTESIAN_POINT('Ctrl Pts',(1.92806066683109E-14,19.9375000013656,
104.958734125));
#4681=CARTESIAN_POINT('Ctrl Pts',(-43.4753311640868,19.8750000013656,104.958734125));
#4682=CARTESIAN_POINT('Ctrl Pts',(-74.2170326445434,19.8125000013656,74.2170326445434));
#4683=CARTESIAN_POINT('Ctrl Pts',(-104.958734125,19.7500000013656,43.4753311640869));
#4684=CARTESIAN_POINT('Ctrl Pts',(-104.958734125,19.6875000013656,0.));
#4685=CARTESIAN_POINT('Ctrl Pts',(-104.958734125,19.6250000013656,-43.4753311640868));
#4686=CARTESIAN_POINT('Ctrl Pts',(-74.2170326445434,19.5625000013656,-74.2170326445434));
#4687=CARTESIAN_POINT('Ctrl Pts',(-43.4753311640868,19.5000000013656,-104.958734125));
#4688=CARTESIAN_POINT('Ctrl Pts',(-6.42686888943697E-15,19.4375000013656,
-104.958734125));
#4689=CARTESIAN_POINT('Ctrl Pts',(43.4753311640868,19.3750000013656,-104.958734125));
#4690=CARTESIAN_POINT('Ctrl Pts',(74.2170326445434,19.3125000013656,-74.2170326445434));
#4691=CARTESIAN_POINT('Ctrl Pts',(104.958734125,19.2500000013656,-43.4753311640868));
#4692=CARTESIAN_POINT('Ctrl Pts',(104.958734125,19.1875000013656,-1.28537377788739E-14));
#4693=CARTESIAN_POINT('Origin',(-7.105427357601E-14,49.5625000013656,-6.0924204042587E-14));
#4694=CARTESIAN_POINT('',(104.958734125,21.1875000013656,-6.0924204042587E-14));
#4695=CARTESIAN_POINT('',(104.958734125,20.9375000013656,-6.0924204042587E-14));
#4696=CARTESIAN_POINT('',(104.958734125,49.5625000013656,-1.089946703063E-13));
#4697=CARTESIAN_POINT('Ctrl Pts',(104.958734125,20.9375000013656,-1.28537377788739E-14));
#4698=CARTESIAN_POINT('Ctrl Pts',(104.958734125,20.8750000013656,43.4753311640868));
#4699=CARTESIAN_POINT('Ctrl Pts',(74.2170326445434,20.8125000013656,74.2170326445434));
#4700=CARTESIAN_POINT('Ctrl Pts',(43.4753311640869,20.7500000013656,104.958734125));
#4701=CARTESIAN_POINT('Ctrl Pts',(1.92806066683109E-14,20.6875000013656,
104.958734125));
#4702=CARTESIAN_POINT('Ctrl Pts',(-43.4753311640868,20.6250000013656,104.958734125));
#4703=CARTESIAN_POINT('Ctrl Pts',(-74.2170326445434,20.5625000013656,74.2170326445434));
#4704=CARTESIAN_POINT('Ctrl Pts',(-104.958734125,20.5000000013656,43.4753311640869));
#4705=CARTESIAN_POINT('Ctrl Pts',(-104.958734125,20.4375000013656,0.));
#4706=CARTESIAN_POINT('Ctrl Pts',(-104.958734125,20.3750000013656,-43.4753311640868));
#4707=CARTESIAN_POINT('Ctrl Pts',(-74.2170326445434,20.3125000013656,-74.2170326445434));
#4708=CARTESIAN_POINT('Ctrl Pts',(-43.4753311640868,20.2500000013656,-104.958734125));
#4709=CARTESIAN_POINT('Ctrl Pts',(-6.42686888943697E-15,20.1875000013656,
-104.958734125));
#4710=CARTESIAN_POINT('Ctrl Pts',(43.4753311640868,20.1250000013656,-104.958734125));
#4711=CARTESIAN_POINT('Ctrl Pts',(74.2170326445434,20.0625000013656,-74.2170326445434));
#4712=CARTESIAN_POINT('Ctrl Pts',(104.958734125,20.0000000013656,-43.4753311640868));
#4713=CARTESIAN_POINT('Ctrl Pts',(104.958734125,19.9375000013656,-1.28537377788739E-14));
#4714=CARTESIAN_POINT('Ctrl Pts',(104.958734125,21.1875000013656,-1.28537377788739E-14));
#4715=CARTESIAN_POINT('Ctrl Pts',(104.958734125,21.1250000013656,43.4753311640868));
#4716=CARTESIAN_POINT('Ctrl Pts',(74.2170326445434,21.0625000013656,74.2170326445434));
#4717=CARTESIAN_POINT('Ctrl Pts',(43.4753311640869,21.0000000013656,104.958734125));
#4718=CARTESIAN_POINT('Ctrl Pts',(1.92806066683109E-14,20.9375000013656,
104.958734125));
#4719=CARTESIAN_POINT('Ctrl Pts',(-43.4753311640868,20.8750000013656,104.958734125));
#4720=CARTESIAN_POINT('Ctrl Pts',(-74.2170326445434,20.8125000013656,74.2170326445434));
#4721=CARTESIAN_POINT('Ctrl Pts',(-104.958734125,20.7500000013656,43.4753311640869));
#4722=CARTESIAN_POINT('Ctrl Pts',(-104.958734125,20.6875000013656,0.));
#4723=CARTESIAN_POINT('Ctrl Pts',(-104.958734125,20.6250000013656,-43.4753311640868));
#4724=CARTESIAN_POINT('Ctrl Pts',(-74.2170326445434,20.5625000013656,-74.2170326445434));
#4725=CARTESIAN_POINT('Ctrl Pts',(-43.4753311640868,20.5000000013656,-104.958734125));
#4726=CARTESIAN_POINT('Ctrl Pts',(-6.42686888943697E-15,20.4375000013656,
-104.958734125));
#4727=CARTESIAN_POINT('Ctrl Pts',(43.4753311640868,20.3750000013656,-104.958734125));
#4728=CARTESIAN_POINT('Ctrl Pts',(74.2170326445434,20.3125000013656,-74.2170326445434));
#4729=CARTESIAN_POINT('Ctrl Pts',(104.958734125,20.2500000013656,-43.4753311640868));
#4730=CARTESIAN_POINT('Ctrl Pts',(104.958734125,20.1875000013656,-1.28537377788739E-14));
#4731=CARTESIAN_POINT('Origin',(-7.105427357601E-14,49.5625000013656,-6.0924204042587E-14));
#4732=CARTESIAN_POINT('',(104.958734125,22.1875000013656,-6.0924204042587E-14));
#4733=CARTESIAN_POINT('',(104.958734125,21.9375000013656,-6.0924204042587E-14));
#4734=CARTESIAN_POINT('',(104.958734125,49.5625000013656,-1.089946703063E-13));
#4735=CARTESIAN_POINT('Ctrl Pts',(104.958734125,21.9375000013656,-1.28537377788739E-14));
#4736=CARTESIAN_POINT('Ctrl Pts',(104.958734125,21.8750000013656,43.4753311640868));
#4737=CARTESIAN_POINT('Ctrl Pts',(74.2170326445434,21.8125000013656,74.2170326445434));
#4738=CARTESIAN_POINT('Ctrl Pts',(43.4753311640869,21.7500000013656,104.958734125));
#4739=CARTESIAN_POINT('Ctrl Pts',(1.92806066683109E-14,21.6875000013656,
104.958734125));
#4740=CARTESIAN_POINT('Ctrl Pts',(-43.4753311640868,21.6250000013656,104.958734125));
#4741=CARTESIAN_POINT('Ctrl Pts',(-74.2170326445434,21.5625000013656,74.2170326445434));
#4742=CARTESIAN_POINT('Ctrl Pts',(-104.958734125,21.5000000013656,43.4753311640869));
#4743=CARTESIAN_POINT('Ctrl Pts',(-104.958734125,21.4375000013656,0.));
#4744=CARTESIAN_POINT('Ctrl Pts',(-104.958734125,21.3750000013656,-43.4753311640868));
#4745=CARTESIAN_POINT('Ctrl Pts',(-74.2170326445434,21.3125000013656,-74.2170326445434));
#4746=CARTESIAN_POINT('Ctrl Pts',(-43.4753311640868,21.2500000013656,-104.958734125));
#4747=CARTESIAN_POINT('Ctrl Pts',(-6.42686888943697E-15,21.1875000013656,
-104.958734125));
#4748=CARTESIAN_POINT('Ctrl Pts',(43.4753311640868,21.1250000013656,-104.958734125));
#4749=CARTESIAN_POINT('Ctrl Pts',(74.2170326445434,21.0625000013656,-74.2170326445434));
#4750=CARTESIAN_POINT('Ctrl Pts',(104.958734125,21.0000000013656,-43.4753311640868));
#4751=CARTESIAN_POINT('Ctrl Pts',(104.958734125,20.9375000013656,-1.28537377788739E-14));
#4752=CARTESIAN_POINT('Ctrl Pts',(104.958734125,22.1875000013656,-1.28537377788739E-14));
#4753=CARTESIAN_POINT('Ctrl Pts',(104.958734125,22.1250000013656,43.4753311640868));
#4754=CARTESIAN_POINT('Ctrl Pts',(74.2170326445434,22.0625000013656,74.2170326445434));
#4755=CARTESIAN_POINT('Ctrl Pts',(43.4753311640869,22.0000000013656,104.958734125));
#4756=CARTESIAN_POINT('Ctrl Pts',(1.92806066683109E-14,21.9375000013656,
104.958734125));
#4757=CARTESIAN_POINT('Ctrl Pts',(-43.4753311640868,21.8750000013656,104.958734125));
#4758=CARTESIAN_POINT('Ctrl Pts',(-74.2170326445434,21.8125000013656,74.2170326445434));
#4759=CARTESIAN_POINT('Ctrl Pts',(-104.958734125,21.7500000013656,43.4753311640869));
#4760=CARTESIAN_POINT('Ctrl Pts',(-104.958734125,21.6875000013656,0.));
#4761=CARTESIAN_POINT('Ctrl Pts',(-104.958734125,21.6250000013656,-43.4753311640868));
#4762=CARTESIAN_POINT('Ctrl Pts',(-74.2170326445434,21.5625000013656,-74.2170326445434));
#4763=CARTESIAN_POINT('Ctrl Pts',(-43.4753311640868,21.5000000013656,-104.958734125));
#4764=CARTESIAN_POINT('Ctrl Pts',(-6.42686888943697E-15,21.4375000013656,
-104.958734125));
#4765=CARTESIAN_POINT('Ctrl Pts',(43.4753311640868,21.3750000013656,-104.958734125));
#4766=CARTESIAN_POINT('Ctrl Pts',(74.2170326445434,21.3125000013656,-74.2170326445434));
#4767=CARTESIAN_POINT('Ctrl Pts',(104.958734125,21.2500000013656,-43.4753311640868));
#4768=CARTESIAN_POINT('Ctrl Pts',(104.958734125,21.1875000013656,-1.28537377788739E-14));
#4769=CARTESIAN_POINT('Origin',(-7.105427357601E-14,49.5625000013656,-6.0924204042587E-14));
#4770=CARTESIAN_POINT('',(104.958734125,23.1875000013656,-6.0924204042587E-14));
#4771=CARTESIAN_POINT('',(104.958734125,22.9375000013656,-6.0924204042587E-14));
#4772=CARTESIAN_POINT('',(104.958734125,49.5625000013656,-1.089946703063E-13));
#4773=CARTESIAN_POINT('Ctrl Pts',(104.958734125,22.9375000013656,-1.28537377788739E-14));
#4774=CARTESIAN_POINT('Ctrl Pts',(104.958734125,22.8750000013656,43.4753311640868));
#4775=CARTESIAN_POINT('Ctrl Pts',(74.2170326445434,22.8125000013656,74.2170326445434));
#4776=CARTESIAN_POINT('Ctrl Pts',(43.4753311640869,22.7500000013656,104.958734125));
#4777=CARTESIAN_POINT('Ctrl Pts',(1.92806066683109E-14,22.6875000013656,
104.958734125));
#4778=CARTESIAN_POINT('Ctrl Pts',(-43.4753311640868,22.6250000013656,104.958734125));
#4779=CARTESIAN_POINT('Ctrl Pts',(-74.2170326445434,22.5625000013656,74.2170326445434));
#4780=CARTESIAN_POINT('Ctrl Pts',(-104.958734125,22.5000000013656,43.4753311640869));
#4781=CARTESIAN_POINT('Ctrl Pts',(-104.958734125,22.4375000013656,0.));
#4782=CARTESIAN_POINT('Ctrl Pts',(-104.958734125,22.3750000013656,-43.4753311640868));
#4783=CARTESIAN_POINT('Ctrl Pts',(-74.2170326445434,22.3125000013656,-74.2170326445434));
#4784=CARTESIAN_POINT('Ctrl Pts',(-43.4753311640868,22.2500000013656,-104.958734125));
#4785=CARTESIAN_POINT('Ctrl Pts',(-6.42686888943697E-15,22.1875000013656,
-104.958734125));
#4786=CARTESIAN_POINT('Ctrl Pts',(43.4753311640868,22.1250000013656,-104.958734125));
#4787=CARTESIAN_POINT('Ctrl Pts',(74.2170326445434,22.0625000013656,-74.2170326445434));
#4788=CARTESIAN_POINT('Ctrl Pts',(104.958734125,22.0000000013656,-43.4753311640868));
#4789=CARTESIAN_POINT('Ctrl Pts',(104.958734125,21.9375000013656,-1.28537377788739E-14));
#4790=CARTESIAN_POINT('Ctrl Pts',(104.958734125,23.1875000013656,-1.28537377788739E-14));
#4791=CARTESIAN_POINT('Ctrl Pts',(104.958734125,23.1250000013656,43.4753311640868));
#4792=CARTESIAN_POINT('Ctrl Pts',(74.2170326445434,23.0625000013656,74.2170326445434));
#4793=CARTESIAN_POINT('Ctrl Pts',(43.4753311640869,23.0000000013656,104.958734125));
#4794=CARTESIAN_POINT('Ctrl Pts',(1.92806066683109E-14,22.9375000013656,
104.958734125));
#4795=CARTESIAN_POINT('Ctrl Pts',(-43.4753311640868,22.8750000013656,104.958734125));
#4796=CARTESIAN_POINT('Ctrl Pts',(-74.2170326445434,22.8125000013656,74.2170326445434));
#4797=CARTESIAN_POINT('Ctrl Pts',(-104.958734125,22.7500000013656,43.4753311640869));
#4798=CARTESIAN_POINT('Ctrl Pts',(-104.958734125,22.6875000013656,0.));
#4799=CARTESIAN_POINT('Ctrl Pts',(-104.958734125,22.6250000013656,-43.4753311640868));
#4800=CARTESIAN_POINT('Ctrl Pts',(-74.2170326445434,22.5625000013656,-74.2170326445434));
#4801=CARTESIAN_POINT('Ctrl Pts',(-43.4753311640868,22.5000000013656,-104.958734125));
#4802=CARTESIAN_POINT('Ctrl Pts',(-6.42686888943697E-15,22.4375000013656,
-104.958734125));
#4803=CARTESIAN_POINT('Ctrl Pts',(43.4753311640868,22.3750000013656,-104.958734125));
#4804=CARTESIAN_POINT('Ctrl Pts',(74.2170326445434,22.3125000013656,-74.2170326445434));
#4805=CARTESIAN_POINT('Ctrl Pts',(104.958734125,22.2500000013656,-43.4753311640868));
#4806=CARTESIAN_POINT('Ctrl Pts',(104.958734125,22.1875000013656,-1.28537377788739E-14));
#4807=CARTESIAN_POINT('Origin',(-7.105427357601E-14,49.5625000013656,-6.0924204042587E-14));
#4808=CARTESIAN_POINT('',(104.958734125,24.1875000013656,-6.0924204042587E-14));
#4809=CARTESIAN_POINT('',(104.958734125,23.9375000013656,-6.0924204042587E-14));
#4810=CARTESIAN_POINT('',(104.958734125,49.5625000013656,-1.089946703063E-13));
#4811=CARTESIAN_POINT('Ctrl Pts',(104.958734125,23.9375000013656,-1.28537377788739E-14));
#4812=CARTESIAN_POINT('Ctrl Pts',(104.958734125,23.8750000013656,43.4753311640868));
#4813=CARTESIAN_POINT('Ctrl Pts',(74.2170326445434,23.8125000013656,74.2170326445434));
#4814=CARTESIAN_POINT('Ctrl Pts',(43.4753311640869,23.7500000013656,104.958734125));
#4815=CARTESIAN_POINT('Ctrl Pts',(1.92806066683109E-14,23.6875000013656,
104.958734125));
#4816=CARTESIAN_POINT('Ctrl Pts',(-43.4753311640868,23.6250000013656,104.958734125));
#4817=CARTESIAN_POINT('Ctrl Pts',(-74.2170326445434,23.5625000013656,74.2170326445434));
#4818=CARTESIAN_POINT('Ctrl Pts',(-104.958734125,23.5000000013656,43.4753311640869));
#4819=CARTESIAN_POINT('Ctrl Pts',(-104.958734125,23.4375000013656,0.));
#4820=CARTESIAN_POINT('Ctrl Pts',(-104.958734125,23.3750000013656,-43.4753311640868));
#4821=CARTESIAN_POINT('Ctrl Pts',(-74.2170326445434,23.3125000013656,-74.2170326445434));
#4822=CARTESIAN_POINT('Ctrl Pts',(-43.4753311640868,23.2500000013656,-104.958734125));
#4823=CARTESIAN_POINT('Ctrl Pts',(-6.42686888943697E-15,23.1875000013656,
-104.958734125));
#4824=CARTESIAN_POINT('Ctrl Pts',(43.4753311640868,23.1250000013656,-104.958734125));
#4825=CARTESIAN_POINT('Ctrl Pts',(74.2170326445434,23.0625000013656,-74.2170326445434));
#4826=CARTESIAN_POINT('Ctrl Pts',(104.958734125,23.0000000013656,-43.4753311640868));
#4827=CARTESIAN_POINT('Ctrl Pts',(104.958734125,22.9375000013656,-1.28537377788739E-14));
#4828=CARTESIAN_POINT('Ctrl Pts',(104.958734125,24.1875000013656,-1.28537377788739E-14));
#4829=CARTESIAN_POINT('Ctrl Pts',(104.958734125,24.1250000013656,43.4753311640868));
#4830=CARTESIAN_POINT('Ctrl Pts',(74.2170326445434,24.0625000013656,74.2170326445434));
#4831=CARTESIAN_POINT('Ctrl Pts',(43.4753311640869,24.0000000013656,104.958734125));
#4832=CARTESIAN_POINT('Ctrl Pts',(1.92806066683109E-14,23.9375000013656,
104.958734125));
#4833=CARTESIAN_POINT('Ctrl Pts',(-43.4753311640868,23.8750000013656,104.958734125));
#4834=CARTESIAN_POINT('Ctrl Pts',(-74.2170326445434,23.8125000013656,74.2170326445434));
#4835=CARTESIAN_POINT('Ctrl Pts',(-104.958734125,23.7500000013656,43.4753311640869));
#4836=CARTESIAN_POINT('Ctrl Pts',(-104.958734125,23.6875000013656,0.));
#4837=CARTESIAN_POINT('Ctrl Pts',(-104.958734125,23.6250000013656,-43.4753311640868));
#4838=CARTESIAN_POINT('Ctrl Pts',(-74.2170326445434,23.5625000013656,-74.2170326445434));
#4839=CARTESIAN_POINT('Ctrl Pts',(-43.4753311640868,23.5000000013656,-104.958734125));
#4840=CARTESIAN_POINT('Ctrl Pts',(-6.42686888943697E-15,23.4375000013656,
-104.958734125));
#4841=CARTESIAN_POINT('Ctrl Pts',(43.4753311640868,23.3750000013656,-104.958734125));
#4842=CARTESIAN_POINT('Ctrl Pts',(74.2170326445434,23.3125000013656,-74.2170326445434));
#4843=CARTESIAN_POINT('Ctrl Pts',(104.958734125,23.2500000013656,-43.4753311640868));
#4844=CARTESIAN_POINT('Ctrl Pts',(104.958734125,23.1875000013656,-1.28537377788739E-14));
#4845=CARTESIAN_POINT('Origin',(-7.105427357601E-14,49.5625000013656,-6.0924204042587E-14));
#4846=CARTESIAN_POINT('',(104.958734125,25.1875000013656,-6.0924204042587E-14));
#4847=CARTESIAN_POINT('',(104.958734125,24.9375000013656,-6.0924204042587E-14));
#4848=CARTESIAN_POINT('',(104.958734125,49.5625000013656,-1.089946703063E-13));
#4849=CARTESIAN_POINT('Ctrl Pts',(104.958734125,24.9375000013656,-1.28537377788739E-14));
#4850=CARTESIAN_POINT('Ctrl Pts',(104.958734125,24.8750000013656,43.4753311640868));
#4851=CARTESIAN_POINT('Ctrl Pts',(74.2170326445434,24.8125000013656,74.2170326445434));
#4852=CARTESIAN_POINT('Ctrl Pts',(43.4753311640869,24.7500000013656,104.958734125));
#4853=CARTESIAN_POINT('Ctrl Pts',(1.92806066683109E-14,24.6875000013656,
104.958734125));
#4854=CARTESIAN_POINT('Ctrl Pts',(-43.4753311640868,24.6250000013656,104.958734125));
#4855=CARTESIAN_POINT('Ctrl Pts',(-74.2170326445434,24.5625000013656,74.2170326445434));
#4856=CARTESIAN_POINT('Ctrl Pts',(-104.958734125,24.5000000013656,43.4753311640869));
#4857=CARTESIAN_POINT('Ctrl Pts',(-104.958734125,24.4375000013656,0.));
#4858=CARTESIAN_POINT('Ctrl Pts',(-104.958734125,24.3750000013656,-43.4753311640868));
#4859=CARTESIAN_POINT('Ctrl Pts',(-74.2170326445434,24.3125000013656,-74.2170326445434));
#4860=CARTESIAN_POINT('Ctrl Pts',(-43.4753311640868,24.2500000013656,-104.958734125));
#4861=CARTESIAN_POINT('Ctrl Pts',(-6.42686888943697E-15,24.1875000013656,
-104.958734125));
#4862=CARTESIAN_POINT('Ctrl Pts',(43.4753311640868,24.1250000013656,-104.958734125));
#4863=CARTESIAN_POINT('Ctrl Pts',(74.2170326445434,24.0625000013656,-74.2170326445434));
#4864=CARTESIAN_POINT('Ctrl Pts',(104.958734125,24.0000000013656,-43.4753311640868));
#4865=CARTESIAN_POINT('Ctrl Pts',(104.958734125,23.9375000013656,-1.28537377788739E-14));
#4866=CARTESIAN_POINT('Ctrl Pts',(104.958734125,25.1875000013656,-1.28537377788739E-14));
#4867=CARTESIAN_POINT('Ctrl Pts',(104.958734125,25.1250000013656,43.4753311640868));
#4868=CARTESIAN_POINT('Ctrl Pts',(74.2170326445434,25.0625000013656,74.2170326445434));
#4869=CARTESIAN_POINT('Ctrl Pts',(43.4753311640869,25.0000000013656,104.958734125));
#4870=CARTESIAN_POINT('Ctrl Pts',(1.92806066683109E-14,24.9375000013656,
104.958734125));
#4871=CARTESIAN_POINT('Ctrl Pts',(-43.4753311640868,24.8750000013656,104.958734125));
#4872=CARTESIAN_POINT('Ctrl Pts',(-74.2170326445434,24.8125000013656,74.2170326445434));
#4873=CARTESIAN_POINT('Ctrl Pts',(-104.958734125,24.7500000013656,43.4753311640869));
#4874=CARTESIAN_POINT('Ctrl Pts',(-104.958734125,24.6875000013656,0.));
#4875=CARTESIAN_POINT('Ctrl Pts',(-104.958734125,24.6250000013656,-43.4753311640868));
#4876=CARTESIAN_POINT('Ctrl Pts',(-74.2170326445434,24.5625000013656,-74.2170326445434));
#4877=CARTESIAN_POINT('Ctrl Pts',(-43.4753311640868,24.5000000013656,-104.958734125));
#4878=CARTESIAN_POINT('Ctrl Pts',(-6.42686888943697E-15,24.4375000013656,
-104.958734125));
#4879=CARTESIAN_POINT('Ctrl Pts',(43.4753311640868,24.3750000013656,-104.958734125));
#4880=CARTESIAN_POINT('Ctrl Pts',(74.2170326445434,24.3125000013656,-74.2170326445434));
#4881=CARTESIAN_POINT('Ctrl Pts',(104.958734125,24.2500000013656,-43.4753311640868));
#4882=CARTESIAN_POINT('Ctrl Pts',(104.958734125,24.1875000013656,-1.28537377788739E-14));
#4883=CARTESIAN_POINT('Origin',(-7.105427357601E-14,49.5625000013656,-6.0924204042587E-14));
#4884=CARTESIAN_POINT('',(104.958734125,26.1875000013656,-6.0924204042587E-14));
#4885=CARTESIAN_POINT('',(104.958734125,25.9375000013656,-6.0924204042587E-14));
#4886=CARTESIAN_POINT('',(104.958734125,49.5625000013656,-1.089946703063E-13));
#4887=CARTESIAN_POINT('Ctrl Pts',(104.958734125,25.9375000013656,-1.28537377788739E-14));
#4888=CARTESIAN_POINT('Ctrl Pts',(104.958734125,25.8750000013656,43.4753311640868));
#4889=CARTESIAN_POINT('Ctrl Pts',(74.2170326445434,25.8125000013656,74.2170326445434));
#4890=CARTESIAN_POINT('Ctrl Pts',(43.4753311640869,25.7500000013656,104.958734125));
#4891=CARTESIAN_POINT('Ctrl Pts',(1.92806066683109E-14,25.6875000013656,
104.958734125));
#4892=CARTESIAN_POINT('Ctrl Pts',(-43.4753311640868,25.6250000013656,104.958734125));
#4893=CARTESIAN_POINT('Ctrl Pts',(-74.2170326445434,25.5625000013656,74.2170326445434));
#4894=CARTESIAN_POINT('Ctrl Pts',(-104.958734125,25.5000000013656,43.4753311640869));
#4895=CARTESIAN_POINT('Ctrl Pts',(-104.958734125,25.4375000013656,0.));
#4896=CARTESIAN_POINT('Ctrl Pts',(-104.958734125,25.3750000013656,-43.4753311640868));
#4897=CARTESIAN_POINT('Ctrl Pts',(-74.2170326445434,25.3125000013656,-74.2170326445434));
#4898=CARTESIAN_POINT('Ctrl Pts',(-43.4753311640868,25.2500000013656,-104.958734125));
#4899=CARTESIAN_POINT('Ctrl Pts',(-6.42686888943697E-15,25.1875000013656,
-104.958734125));
#4900=CARTESIAN_POINT('Ctrl Pts',(43.4753311640868,25.1250000013656,-104.958734125));
#4901=CARTESIAN_POINT('Ctrl Pts',(74.2170326445434,25.0625000013656,-74.2170326445434));
#4902=CARTESIAN_POINT('Ctrl Pts',(104.958734125,25.0000000013656,-43.4753311640868));
#4903=CARTESIAN_POINT('Ctrl Pts',(104.958734125,24.9375000013656,-1.28537377788739E-14));
#4904=CARTESIAN_POINT('Ctrl Pts',(104.958734125,26.1875000013656,-1.28537377788739E-14));
#4905=CARTESIAN_POINT('Ctrl Pts',(104.958734125,26.1250000013656,43.4753311640868));
#4906=CARTESIAN_POINT('Ctrl Pts',(74.2170326445434,26.0625000013656,74.2170326445434));
#4907=CARTESIAN_POINT('Ctrl Pts',(43.4753311640869,26.0000000013656,104.958734125));
#4908=CARTESIAN_POINT('Ctrl Pts',(1.92806066683109E-14,25.9375000013656,
104.958734125));
#4909=CARTESIAN_POINT('Ctrl Pts',(-43.4753311640868,25.8750000013656,104.958734125));
#4910=CARTESIAN_POINT('Ctrl Pts',(-74.2170326445434,25.8125000013656,74.2170326445434));
#4911=CARTESIAN_POINT('Ctrl Pts',(-104.958734125,25.7500000013656,43.4753311640869));
#4912=CARTESIAN_POINT('Ctrl Pts',(-104.958734125,25.6875000013656,0.));
#4913=CARTESIAN_POINT('Ctrl Pts',(-104.958734125,25.6250000013656,-43.4753311640868));
#4914=CARTESIAN_POINT('Ctrl Pts',(-74.2170326445434,25.5625000013656,-74.2170326445434));
#4915=CARTESIAN_POINT('Ctrl Pts',(-43.4753311640868,25.5000000013656,-104.958734125));
#4916=CARTESIAN_POINT('Ctrl Pts',(-6.42686888943697E-15,25.4375000013656,
-104.958734125));
#4917=CARTESIAN_POINT('Ctrl Pts',(43.4753311640868,25.3750000013656,-104.958734125));
#4918=CARTESIAN_POINT('Ctrl Pts',(74.2170326445434,25.3125000013656,-74.2170326445434));
#4919=CARTESIAN_POINT('Ctrl Pts',(104.958734125,25.2500000013656,-43.4753311640868));
#4920=CARTESIAN_POINT('Ctrl Pts',(104.958734125,25.1875000013656,-1.28537377788739E-14));
#4921=CARTESIAN_POINT('Origin',(-7.105427357601E-14,49.5625000013656,-6.0924204042587E-14));
#4922=CARTESIAN_POINT('',(104.958734125,27.1875000013656,-6.0924204042587E-14));
#4923=CARTESIAN_POINT('',(104.958734125,26.9375000013656,-6.0924204042587E-14));
#4924=CARTESIAN_POINT('',(104.958734125,49.5625000013656,-1.089946703063E-13));
#4925=CARTESIAN_POINT('Ctrl Pts',(104.958734125,26.9375000013656,-1.28537377788739E-14));
#4926=CARTESIAN_POINT('Ctrl Pts',(104.958734125,26.8750000013656,43.4753311640868));
#4927=CARTESIAN_POINT('Ctrl Pts',(74.2170326445434,26.8125000013656,74.2170326445434));
#4928=CARTESIAN_POINT('Ctrl Pts',(43.4753311640869,26.7500000013656,104.958734125));
#4929=CARTESIAN_POINT('Ctrl Pts',(1.92806066683109E-14,26.6875000013656,
104.958734125));
#4930=CARTESIAN_POINT('Ctrl Pts',(-43.4753311640868,26.6250000013656,104.958734125));
#4931=CARTESIAN_POINT('Ctrl Pts',(-74.2170326445434,26.5625000013656,74.2170326445434));
#4932=CARTESIAN_POINT('Ctrl Pts',(-104.958734125,26.5000000013656,43.4753311640869));
#4933=CARTESIAN_POINT('Ctrl Pts',(-104.958734125,26.4375000013656,0.));
#4934=CARTESIAN_POINT('Ctrl Pts',(-104.958734125,26.3750000013656,-43.4753311640868));
#4935=CARTESIAN_POINT('Ctrl Pts',(-74.2170326445434,26.3125000013656,-74.2170326445434));
#4936=CARTESIAN_POINT('Ctrl Pts',(-43.4753311640868,26.2500000013656,-104.958734125));
#4937=CARTESIAN_POINT('Ctrl Pts',(-6.42686888943697E-15,26.1875000013656,
-104.958734125));
#4938=CARTESIAN_POINT('Ctrl Pts',(43.4753311640868,26.1250000013656,-104.958734125));
#4939=CARTESIAN_POINT('Ctrl Pts',(74.2170326445434,26.0625000013656,-74.2170326445434));
#4940=CARTESIAN_POINT('Ctrl Pts',(104.958734125,26.0000000013656,-43.4753311640868));
#4941=CARTESIAN_POINT('Ctrl Pts',(104.958734125,25.9375000013656,-1.28537377788739E-14));
#4942=CARTESIAN_POINT('Ctrl Pts',(104.958734125,27.1875000013656,-1.28537377788739E-14));
#4943=CARTESIAN_POINT('Ctrl Pts',(104.958734125,27.1250000013656,43.4753311640868));
#4944=CARTESIAN_POINT('Ctrl Pts',(74.2170326445434,27.0625000013656,74.2170326445434));
#4945=CARTESIAN_POINT('Ctrl Pts',(43.4753311640869,27.0000000013656,104.958734125));
#4946=CARTESIAN_POINT('Ctrl Pts',(1.92806066683109E-14,26.9375000013656,
104.958734125));
#4947=CARTESIAN_POINT('Ctrl Pts',(-43.4753311640868,26.8750000013656,104.958734125));
#4948=CARTESIAN_POINT('Ctrl Pts',(-74.2170326445434,26.8125000013656,74.2170326445434));
#4949=CARTESIAN_POINT('Ctrl Pts',(-104.958734125,26.7500000013656,43.4753311640869));
#4950=CARTESIAN_POINT('Ctrl Pts',(-104.958734125,26.6875000013656,0.));
#4951=CARTESIAN_POINT('Ctrl Pts',(-104.958734125,26.6250000013656,-43.4753311640868));
#4952=CARTESIAN_POINT('Ctrl Pts',(-74.2170326445434,26.5625000013656,-74.2170326445434));
#4953=CARTESIAN_POINT('Ctrl Pts',(-43.4753311640868,26.5000000013656,-104.958734125));
#4954=CARTESIAN_POINT('Ctrl Pts',(-6.42686888943697E-15,26.4375000013656,
-104.958734125));
#4955=CARTESIAN_POINT('Ctrl Pts',(43.4753311640868,26.3750000013656,-104.958734125));
#4956=CARTESIAN_POINT('Ctrl Pts',(74.2170326445434,26.3125000013656,-74.2170326445434));
#4957=CARTESIAN_POINT('Ctrl Pts',(104.958734125,26.2500000013656,-43.4753311640868));
#4958=CARTESIAN_POINT('Ctrl Pts',(104.958734125,26.1875000013656,-1.28537377788739E-14));
#4959=CARTESIAN_POINT('Origin',(-7.105427357601E-14,49.5625000013656,-6.0924204042587E-14));
#4960=CARTESIAN_POINT('',(104.958734125,28.1875000013656,-6.0924204042587E-14));
#4961=CARTESIAN_POINT('',(104.958734125,27.9375000013656,-6.0924204042587E-14));
#4962=CARTESIAN_POINT('',(104.958734125,49.5625000013656,-1.089946703063E-13));
#4963=CARTESIAN_POINT('Ctrl Pts',(104.958734125,27.9375000013656,-1.28537377788739E-14));
#4964=CARTESIAN_POINT('Ctrl Pts',(104.958734125,27.8750000013656,43.4753311640868));
#4965=CARTESIAN_POINT('Ctrl Pts',(74.2170326445434,27.8125000013656,74.2170326445434));
#4966=CARTESIAN_POINT('Ctrl Pts',(43.4753311640869,27.7500000013656,104.958734125));
#4967=CARTESIAN_POINT('Ctrl Pts',(1.92806066683109E-14,27.6875000013656,
104.958734125));
#4968=CARTESIAN_POINT('Ctrl Pts',(-43.4753311640868,27.6250000013656,104.958734125));
#4969=CARTESIAN_POINT('Ctrl Pts',(-74.2170326445434,27.5625000013656,74.2170326445434));
#4970=CARTESIAN_POINT('Ctrl Pts',(-104.958734125,27.5000000013656,43.4753311640869));
#4971=CARTESIAN_POINT('Ctrl Pts',(-104.958734125,27.4375000013656,0.));
#4972=CARTESIAN_POINT('Ctrl Pts',(-104.958734125,27.3750000013656,-43.4753311640868));
#4973=CARTESIAN_POINT('Ctrl Pts',(-74.2170326445434,27.3125000013656,-74.2170326445434));
#4974=CARTESIAN_POINT('Ctrl Pts',(-43.4753311640868,27.2500000013656,-104.958734125));
#4975=CARTESIAN_POINT('Ctrl Pts',(-6.42686888943697E-15,27.1875000013656,
-104.958734125));
#4976=CARTESIAN_POINT('Ctrl Pts',(43.4753311640868,27.1250000013656,-104.958734125));
#4977=CARTESIAN_POINT('Ctrl Pts',(74.2170326445434,27.0625000013656,-74.2170326445434));
#4978=CARTESIAN_POINT('Ctrl Pts',(104.958734125,27.0000000013656,-43.4753311640868));
#4979=CARTESIAN_POINT('Ctrl Pts',(104.958734125,26.9375000013656,-1.28537377788739E-14));
#4980=CARTESIAN_POINT('Ctrl Pts',(104.958734125,28.1875000013656,-1.28537377788739E-14));
#4981=CARTESIAN_POINT('Ctrl Pts',(104.958734125,28.1250000013656,43.4753311640868));
#4982=CARTESIAN_POINT('Ctrl Pts',(74.2170326445434,28.0625000013656,74.2170326445434));
#4983=CARTESIAN_POINT('Ctrl Pts',(43.4753311640869,28.0000000013656,104.958734125));
#4984=CARTESIAN_POINT('Ctrl Pts',(1.92806066683109E-14,27.9375000013656,
104.958734125));
#4985=CARTESIAN_POINT('Ctrl Pts',(-43.4753311640868,27.8750000013656,104.958734125));
#4986=CARTESIAN_POINT('Ctrl Pts',(-74.2170326445434,27.8125000013656,74.2170326445434));
#4987=CARTESIAN_POINT('Ctrl Pts',(-104.958734125,27.7500000013656,43.4753311640869));
#4988=CARTESIAN_POINT('Ctrl Pts',(-104.958734125,27.6875000013656,0.));
#4989=CARTESIAN_POINT('Ctrl Pts',(-104.958734125,27.6250000013656,-43.4753311640868));
#4990=CARTESIAN_POINT('Ctrl Pts',(-74.2170326445434,27.5625000013656,-74.2170326445434));
#4991=CARTESIAN_POINT('Ctrl Pts',(-43.4753311640868,27.5000000013656,-104.958734125));
#4992=CARTESIAN_POINT('Ctrl Pts',(-6.42686888943697E-15,27.4375000013656,
-104.958734125));
#4993=CARTESIAN_POINT('Ctrl Pts',(43.4753311640868,27.3750000013656,-104.958734125));
#4994=CARTESIAN_POINT('Ctrl Pts',(74.2170326445434,27.3125000013656,-74.2170326445434));
#4995=CARTESIAN_POINT('Ctrl Pts',(104.958734125,27.2500000013656,-43.4753311640868));
#4996=CARTESIAN_POINT('Ctrl Pts',(104.958734125,27.1875000013656,-1.28537377788739E-14));
#4997=CARTESIAN_POINT('Origin',(-7.105427357601E-14,49.5625000013656,-6.0924204042587E-14));
#4998=CARTESIAN_POINT('',(104.958734125,29.1875000013656,-6.0924204042587E-14));
#4999=CARTESIAN_POINT('',(104.958734125,28.9375000013656,-6.0924204042587E-14));
#5000=CARTESIAN_POINT('',(104.958734125,49.5625000013656,-1.089946703063E-13));
#5001=CARTESIAN_POINT('Ctrl Pts',(104.958734125,28.9375000013656,-1.28537377788739E-14));
#5002=CARTESIAN_POINT('Ctrl Pts',(104.958734125,28.8750000013656,43.4753311640868));
#5003=CARTESIAN_POINT('Ctrl Pts',(74.2170326445434,28.8125000013656,74.2170326445434));
#5004=CARTESIAN_POINT('Ctrl Pts',(43.4753311640869,28.7500000013656,104.958734125));
#5005=CARTESIAN_POINT('Ctrl Pts',(1.92806066683109E-14,28.6875000013656,
104.958734125));
#5006=CARTESIAN_POINT('Ctrl Pts',(-43.4753311640868,28.6250000013656,104.958734125));
#5007=CARTESIAN_POINT('Ctrl Pts',(-74.2170326445434,28.5625000013656,74.2170326445434));
#5008=CARTESIAN_POINT('Ctrl Pts',(-104.958734125,28.5000000013656,43.4753311640869));
#5009=CARTESIAN_POINT('Ctrl Pts',(-104.958734125,28.4375000013656,0.));
#5010=CARTESIAN_POINT('Ctrl Pts',(-104.958734125,28.3750000013656,-43.4753311640868));
#5011=CARTESIAN_POINT('Ctrl Pts',(-74.2170326445434,28.3125000013656,-74.2170326445434));
#5012=CARTESIAN_POINT('Ctrl Pts',(-43.4753311640868,28.2500000013656,-104.958734125));
#5013=CARTESIAN_POINT('Ctrl Pts',(-6.42686888943697E-15,28.1875000013656,
-104.958734125));
#5014=CARTESIAN_POINT('Ctrl Pts',(43.4753311640868,28.1250000013656,-104.958734125));
#5015=CARTESIAN_POINT('Ctrl Pts',(74.2170326445434,28.0625000013656,-74.2170326445434));
#5016=CARTESIAN_POINT('Ctrl Pts',(104.958734125,28.0000000013656,-43.4753311640868));
#5017=CARTESIAN_POINT('Ctrl Pts',(104.958734125,27.9375000013656,-1.28537377788739E-14));
#5018=CARTESIAN_POINT('Ctrl Pts',(104.958734125,29.1875000013656,-1.28537377788739E-14));
#5019=CARTESIAN_POINT('Ctrl Pts',(104.958734125,29.1250000013656,43.4753311640868));
#5020=CARTESIAN_POINT('Ctrl Pts',(74.2170326445434,29.0625000013656,74.2170326445434));
#5021=CARTESIAN_POINT('Ctrl Pts',(43.4753311640869,29.0000000013656,104.958734125));
#5022=CARTESIAN_POINT('Ctrl Pts',(1.92806066683109E-14,28.9375000013656,
104.958734125));
#5023=CARTESIAN_POINT('Ctrl Pts',(-43.4753311640868,28.8750000013656,104.958734125));
#5024=CARTESIAN_POINT('Ctrl Pts',(-74.2170326445434,28.8125000013656,74.2170326445434));
#5025=CARTESIAN_POINT('Ctrl Pts',(-104.958734125,28.7500000013656,43.4753311640869));
#5026=CARTESIAN_POINT('Ctrl Pts',(-104.958734125,28.6875000013656,0.));
#5027=CARTESIAN_POINT('Ctrl Pts',(-104.958734125,28.6250000013656,-43.4753311640868));
#5028=CARTESIAN_POINT('Ctrl Pts',(-74.2170326445434,28.5625000013656,-74.2170326445434));
#5029=CARTESIAN_POINT('Ctrl Pts',(-43.4753311640868,28.5000000013656,-104.958734125));
#5030=CARTESIAN_POINT('Ctrl Pts',(-6.42686888943697E-15,28.4375000013656,
-104.958734125));
#5031=CARTESIAN_POINT('Ctrl Pts',(43.4753311640868,28.3750000013656,-104.958734125));
#5032=CARTESIAN_POINT('Ctrl Pts',(74.2170326445434,28.3125000013656,-74.2170326445434));
#5033=CARTESIAN_POINT('Ctrl Pts',(104.958734125,28.2500000013656,-43.4753311640868));
#5034=CARTESIAN_POINT('Ctrl Pts',(104.958734125,28.1875000013656,-1.28537377788739E-14));
#5035=CARTESIAN_POINT('Origin',(-7.105427357601E-14,49.5625000013656,-6.0924204042587E-14));
#5036=CARTESIAN_POINT('',(104.958734125,30.1875000013656,-6.0924204042587E-14));
#5037=CARTESIAN_POINT('',(104.958734125,29.9375000013656,-6.0924204042587E-14));
#5038=CARTESIAN_POINT('',(104.958734125,49.5625000013656,-1.089946703063E-13));
#5039=CARTESIAN_POINT('Ctrl Pts',(104.958734125,29.9375000013656,-1.28537377788739E-14));
#5040=CARTESIAN_POINT('Ctrl Pts',(104.958734125,29.8750000013656,43.4753311640868));
#5041=CARTESIAN_POINT('Ctrl Pts',(74.2170326445434,29.8125000013656,74.2170326445434));
#5042=CARTESIAN_POINT('Ctrl Pts',(43.4753311640869,29.7500000013656,104.958734125));
#5043=CARTESIAN_POINT('Ctrl Pts',(1.92806066683109E-14,29.6875000013656,
104.958734125));
#5044=CARTESIAN_POINT('Ctrl Pts',(-43.4753311640868,29.6250000013656,104.958734125));
#5045=CARTESIAN_POINT('Ctrl Pts',(-74.2170326445434,29.5625000013656,74.2170326445434));
#5046=CARTESIAN_POINT('Ctrl Pts',(-104.958734125,29.5000000013656,43.4753311640869));
#5047=CARTESIAN_POINT('Ctrl Pts',(-104.958734125,29.4375000013656,0.));
#5048=CARTESIAN_POINT('Ctrl Pts',(-104.958734125,29.3750000013656,-43.4753311640868));
#5049=CARTESIAN_POINT('Ctrl Pts',(-74.2170326445434,29.3125000013656,-74.2170326445434));
#5050=CARTESIAN_POINT('Ctrl Pts',(-43.4753311640868,29.2500000013656,-104.958734125));
#5051=CARTESIAN_POINT('Ctrl Pts',(-6.42686888943697E-15,29.1875000013656,
-104.958734125));
#5052=CARTESIAN_POINT('Ctrl Pts',(43.4753311640868,29.1250000013656,-104.958734125));
#5053=CARTESIAN_POINT('Ctrl Pts',(74.2170326445434,29.0625000013656,-74.2170326445434));
#5054=CARTESIAN_POINT('Ctrl Pts',(104.958734125,29.0000000013656,-43.4753311640868));
#5055=CARTESIAN_POINT('Ctrl Pts',(104.958734125,28.9375000013656,-1.28537377788739E-14));
#5056=CARTESIAN_POINT('Ctrl Pts',(104.958734125,30.1875000013656,-1.28537377788739E-14));
#5057=CARTESIAN_POINT('Ctrl Pts',(104.958734125,30.1250000013656,43.4753311640868));
#5058=CARTESIAN_POINT('Ctrl Pts',(74.2170326445434,30.0625000013656,74.2170326445434));
#5059=CARTESIAN_POINT('Ctrl Pts',(43.4753311640869,30.0000000013656,104.958734125));
#5060=CARTESIAN_POINT('Ctrl Pts',(1.92806066683109E-14,29.9375000013656,
104.958734125));
#5061=CARTESIAN_POINT('Ctrl Pts',(-43.4753311640868,29.8750000013656,104.958734125));
#5062=CARTESIAN_POINT('Ctrl Pts',(-74.2170326445434,29.8125000013656,74.2170326445434));
#5063=CARTESIAN_POINT('Ctrl Pts',(-104.958734125,29.7500000013656,43.4753311640869));
#5064=CARTESIAN_POINT('Ctrl Pts',(-104.958734125,29.6875000013656,0.));
#5065=CARTESIAN_POINT('Ctrl Pts',(-104.958734125,29.6250000013656,-43.4753311640868));
#5066=CARTESIAN_POINT('Ctrl Pts',(-74.2170326445434,29.5625000013656,-74.2170326445434));
#5067=CARTESIAN_POINT('Ctrl Pts',(-43.4753311640868,29.5000000013656,-104.958734125));
#5068=CARTESIAN_POINT('Ctrl Pts',(-6.42686888943697E-15,29.4375000013656,
-104.958734125));
#5069=CARTESIAN_POINT('Ctrl Pts',(43.4753311640868,29.3750000013656,-104.958734125));
#5070=CARTESIAN_POINT('Ctrl Pts',(74.2170326445434,29.3125000013656,-74.2170326445434));
#5071=CARTESIAN_POINT('Ctrl Pts',(104.958734125,29.2500000013656,-43.4753311640868));
#5072=CARTESIAN_POINT('Ctrl Pts',(104.958734125,29.1875000013656,-1.28537377788739E-14));
#5073=CARTESIAN_POINT('Origin',(-7.105427357601E-14,49.5625000013656,-6.0924204042587E-14));
#5074=CARTESIAN_POINT('',(104.958734125,31.1875000013656,-6.0924204042587E-14));
#5075=CARTESIAN_POINT('',(104.958734125,30.9375000013656,-6.0924204042587E-14));
#5076=CARTESIAN_POINT('',(104.958734125,49.5625000013656,-1.089946703063E-13));
#5077=CARTESIAN_POINT('Ctrl Pts',(104.958734125,30.9375000013656,-1.28537377788739E-14));
#5078=CARTESIAN_POINT('Ctrl Pts',(104.958734125,30.8750000013656,43.4753311640868));
#5079=CARTESIAN_POINT('Ctrl Pts',(74.2170326445434,30.8125000013656,74.2170326445434));
#5080=CARTESIAN_POINT('Ctrl Pts',(43.4753311640869,30.7500000013656,104.958734125));
#5081=CARTESIAN_POINT('Ctrl Pts',(1.92806066683109E-14,30.6875000013656,
104.958734125));
#5082=CARTESIAN_POINT('Ctrl Pts',(-43.4753311640868,30.6250000013656,104.958734125));
#5083=CARTESIAN_POINT('Ctrl Pts',(-74.2170326445434,30.5625000013656,74.2170326445434));
#5084=CARTESIAN_POINT('Ctrl Pts',(-104.958734125,30.5000000013656,43.4753311640869));
#5085=CARTESIAN_POINT('Ctrl Pts',(-104.958734125,30.4375000013656,0.));
#5086=CARTESIAN_POINT('Ctrl Pts',(-104.958734125,30.3750000013656,-43.4753311640868));
#5087=CARTESIAN_POINT('Ctrl Pts',(-74.2170326445434,30.3125000013656,-74.2170326445434));
#5088=CARTESIAN_POINT('Ctrl Pts',(-43.4753311640868,30.2500000013656,-104.958734125));
#5089=CARTESIAN_POINT('Ctrl Pts',(-6.42686888943697E-15,30.1875000013656,
-104.958734125));
#5090=CARTESIAN_POINT('Ctrl Pts',(43.4753311640868,30.1250000013656,-104.958734125));
#5091=CARTESIAN_POINT('Ctrl Pts',(74.2170326445434,30.0625000013656,-74.2170326445434));
#5092=CARTESIAN_POINT('Ctrl Pts',(104.958734125,30.0000000013656,-43.4753311640868));
#5093=CARTESIAN_POINT('Ctrl Pts',(104.958734125,29.9375000013656,-1.28537377788739E-14));
#5094=CARTESIAN_POINT('Ctrl Pts',(104.958734125,31.1875000013656,-1.28537377788739E-14));
#5095=CARTESIAN_POINT('Ctrl Pts',(104.958734125,31.1250000013656,43.4753311640868));
#5096=CARTESIAN_POINT('Ctrl Pts',(74.2170326445434,31.0625000013656,74.2170326445434));
#5097=CARTESIAN_POINT('Ctrl Pts',(43.4753311640869,31.0000000013656,104.958734125));
#5098=CARTESIAN_POINT('Ctrl Pts',(1.92806066683109E-14,30.9375000013656,
104.958734125));
#5099=CARTESIAN_POINT('Ctrl Pts',(-43.4753311640868,30.8750000013656,104.958734125));
#5100=CARTESIAN_POINT('Ctrl Pts',(-74.2170326445434,30.8125000013656,74.2170326445434));
#5101=CARTESIAN_POINT('Ctrl Pts',(-104.958734125,30.7500000013656,43.4753311640869));
#5102=CARTESIAN_POINT('Ctrl Pts',(-104.958734125,30.6875000013656,0.));
#5103=CARTESIAN_POINT('Ctrl Pts',(-104.958734125,30.6250000013656,-43.4753311640868));
#5104=CARTESIAN_POINT('Ctrl Pts',(-74.2170326445434,30.5625000013656,-74.2170326445434));
#5105=CARTESIAN_POINT('Ctrl Pts',(-43.4753311640868,30.5000000013656,-104.958734125));
#5106=CARTESIAN_POINT('Ctrl Pts',(-6.42686888943697E-15,30.4375000013656,
-104.958734125));
#5107=CARTESIAN_POINT('Ctrl Pts',(43.4753311640868,30.3750000013656,-104.958734125));
#5108=CARTESIAN_POINT('Ctrl Pts',(74.2170326445434,30.3125000013656,-74.2170326445434));
#5109=CARTESIAN_POINT('Ctrl Pts',(104.958734125,30.2500000013656,-43.4753311640868));
#5110=CARTESIAN_POINT('Ctrl Pts',(104.958734125,30.1875000013656,-1.28537377788739E-14));
#5111=CARTESIAN_POINT('Origin',(-7.105427357601E-14,49.5625000013656,-6.0924204042587E-14));
#5112=CARTESIAN_POINT('',(104.958734125,32.1875000013656,-6.0924204042587E-14));
#5113=CARTESIAN_POINT('',(104.958734125,31.9375000013656,-6.0924204042587E-14));
#5114=CARTESIAN_POINT('',(104.958734125,49.5625000013656,-1.089946703063E-13));
#5115=CARTESIAN_POINT('Ctrl Pts',(104.958734125,31.9375000013656,-1.28537377788739E-14));
#5116=CARTESIAN_POINT('Ctrl Pts',(104.958734125,31.8750000013656,43.4753311640868));
#5117=CARTESIAN_POINT('Ctrl Pts',(74.2170326445434,31.8125000013656,74.2170326445434));
#5118=CARTESIAN_POINT('Ctrl Pts',(43.4753311640869,31.7500000013656,104.958734125));
#5119=CARTESIAN_POINT('Ctrl Pts',(1.92806066683109E-14,31.6875000013656,
104.958734125));
#5120=CARTESIAN_POINT('Ctrl Pts',(-43.4753311640868,31.6250000013656,104.958734125));
#5121=CARTESIAN_POINT('Ctrl Pts',(-74.2170326445434,31.5625000013656,74.2170326445434));
#5122=CARTESIAN_POINT('Ctrl Pts',(-104.958734125,31.5000000013656,43.4753311640869));
#5123=CARTESIAN_POINT('Ctrl Pts',(-104.958734125,31.4375000013656,0.));
#5124=CARTESIAN_POINT('Ctrl Pts',(-104.958734125,31.3750000013656,-43.4753311640868));
#5125=CARTESIAN_POINT('Ctrl Pts',(-74.2170326445434,31.3125000013656,-74.2170326445434));
#5126=CARTESIAN_POINT('Ctrl Pts',(-43.4753311640868,31.2500000013656,-104.958734125));
#5127=CARTESIAN_POINT('Ctrl Pts',(-6.42686888943697E-15,31.1875000013656,
-104.958734125));
#5128=CARTESIAN_POINT('Ctrl Pts',(43.4753311640868,31.1250000013656,-104.958734125));
#5129=CARTESIAN_POINT('Ctrl Pts',(74.2170326445434,31.0625000013656,-74.2170326445434));
#5130=CARTESIAN_POINT('Ctrl Pts',(104.958734125,31.0000000013656,-43.4753311640868));
#5131=CARTESIAN_POINT('Ctrl Pts',(104.958734125,30.9375000013656,-1.28537377788739E-14));
#5132=CARTESIAN_POINT('Ctrl Pts',(104.958734125,32.1875000013656,-1.28537377788739E-14));
#5133=CARTESIAN_POINT('Ctrl Pts',(104.958734125,32.1250000013656,43.4753311640868));
#5134=CARTESIAN_POINT('Ctrl Pts',(74.2170326445434,32.0625000013656,74.2170326445434));
#5135=CARTESIAN_POINT('Ctrl Pts',(43.4753311640869,32.0000000013656,104.958734125));
#5136=CARTESIAN_POINT('Ctrl Pts',(1.92806066683109E-14,31.9375000013656,
104.958734125));
#5137=CARTESIAN_POINT('Ctrl Pts',(-43.4753311640868,31.8750000013656,104.958734125));
#5138=CARTESIAN_POINT('Ctrl Pts',(-74.2170326445434,31.8125000013656,74.2170326445434));
#5139=CARTESIAN_POINT('Ctrl Pts',(-104.958734125,31.7500000013656,43.4753311640869));
#5140=CARTESIAN_POINT('Ctrl Pts',(-104.958734125,31.6875000013656,0.));
#5141=CARTESIAN_POINT('Ctrl Pts',(-104.958734125,31.6250000013656,-43.4753311640868));
#5142=CARTESIAN_POINT('Ctrl Pts',(-74.2170326445434,31.5625000013656,-74.2170326445434));
#5143=CARTESIAN_POINT('Ctrl Pts',(-43.4753311640868,31.5000000013656,-104.958734125));
#5144=CARTESIAN_POINT('Ctrl Pts',(-6.42686888943697E-15,31.4375000013656,
-104.958734125));
#5145=CARTESIAN_POINT('Ctrl Pts',(43.4753311640868,31.3750000013656,-104.958734125));
#5146=CARTESIAN_POINT('Ctrl Pts',(74.2170326445434,31.3125000013656,-74.2170326445434));
#5147=CARTESIAN_POINT('Ctrl Pts',(104.958734125,31.2500000013656,-43.4753311640868));
#5148=CARTESIAN_POINT('Ctrl Pts',(104.958734125,31.1875000013656,-1.28537377788739E-14));
#5149=CARTESIAN_POINT('Origin',(-7.105427357601E-14,49.5625000013656,-6.0924204042587E-14));
#5150=CARTESIAN_POINT('',(104.958734125,33.1875000013656,-6.0924204042587E-14));
#5151=CARTESIAN_POINT('',(104.958734125,32.9375000013656,-6.0924204042587E-14));
#5152=CARTESIAN_POINT('',(104.958734125,49.5625000013656,-1.089946703063E-13));
#5153=CARTESIAN_POINT('Ctrl Pts',(104.958734125,32.9375000013656,-1.28537377788739E-14));
#5154=CARTESIAN_POINT('Ctrl Pts',(104.958734125,32.8750000013656,43.4753311640868));
#5155=CARTESIAN_POINT('Ctrl Pts',(74.2170326445434,32.8125000013656,74.2170326445434));
#5156=CARTESIAN_POINT('Ctrl Pts',(43.4753311640869,32.7500000013656,104.958734125));
#5157=CARTESIAN_POINT('Ctrl Pts',(1.92806066683109E-14,32.6875000013656,
104.958734125));
#5158=CARTESIAN_POINT('Ctrl Pts',(-43.4753311640868,32.6250000013656,104.958734125));
#5159=CARTESIAN_POINT('Ctrl Pts',(-74.2170326445434,32.5625000013656,74.2170326445434));
#5160=CARTESIAN_POINT('Ctrl Pts',(-104.958734125,32.5000000013656,43.4753311640869));
#5161=CARTESIAN_POINT('Ctrl Pts',(-104.958734125,32.4375000013656,0.));
#5162=CARTESIAN_POINT('Ctrl Pts',(-104.958734125,32.3750000013656,-43.4753311640868));
#5163=CARTESIAN_POINT('Ctrl Pts',(-74.2170326445434,32.3125000013656,-74.2170326445434));
#5164=CARTESIAN_POINT('Ctrl Pts',(-43.4753311640868,32.2500000013656,-104.958734125));
#5165=CARTESIAN_POINT('Ctrl Pts',(-6.42686888943697E-15,32.1875000013656,
-104.958734125));
#5166=CARTESIAN_POINT('Ctrl Pts',(43.4753311640868,32.1250000013656,-104.958734125));
#5167=CARTESIAN_POINT('Ctrl Pts',(74.2170326445434,32.0625000013656,-74.2170326445434));
#5168=CARTESIAN_POINT('Ctrl Pts',(104.958734125,32.0000000013656,-43.4753311640868));
#5169=CARTESIAN_POINT('Ctrl Pts',(104.958734125,31.9375000013656,-1.28537377788739E-14));
#5170=CARTESIAN_POINT('Ctrl Pts',(104.958734125,33.1875000013656,-1.28537377788739E-14));
#5171=CARTESIAN_POINT('Ctrl Pts',(104.958734125,33.1250000013656,43.4753311640868));
#5172=CARTESIAN_POINT('Ctrl Pts',(74.2170326445434,33.0625000013656,74.2170326445434));
#5173=CARTESIAN_POINT('Ctrl Pts',(43.4753311640869,33.0000000013656,104.958734125));
#5174=CARTESIAN_POINT('Ctrl Pts',(1.92806066683109E-14,32.9375000013656,
104.958734125));
#5175=CARTESIAN_POINT('Ctrl Pts',(-43.4753311640868,32.8750000013656,104.958734125));
#5176=CARTESIAN_POINT('Ctrl Pts',(-74.2170326445434,32.8125000013656,74.2170326445434));
#5177=CARTESIAN_POINT('Ctrl Pts',(-104.958734125,32.7500000013656,43.4753311640869));
#5178=CARTESIAN_POINT('Ctrl Pts',(-104.958734125,32.6875000013656,0.));
#5179=CARTESIAN_POINT('Ctrl Pts',(-104.958734125,32.6250000013656,-43.4753311640868));
#5180=CARTESIAN_POINT('Ctrl Pts',(-74.2170326445434,32.5625000013656,-74.2170326445434));
#5181=CARTESIAN_POINT('Ctrl Pts',(-43.4753311640868,32.5000000013656,-104.958734125));
#5182=CARTESIAN_POINT('Ctrl Pts',(-6.42686888943697E-15,32.4375000013656,
-104.958734125));
#5183=CARTESIAN_POINT('Ctrl Pts',(43.4753311640868,32.3750000013656,-104.958734125));
#5184=CARTESIAN_POINT('Ctrl Pts',(74.2170326445434,32.3125000013656,-74.2170326445434));
#5185=CARTESIAN_POINT('Ctrl Pts',(104.958734125,32.2500000013656,-43.4753311640868));
#5186=CARTESIAN_POINT('Ctrl Pts',(104.958734125,32.1875000013656,-1.28537377788739E-14));
#5187=CARTESIAN_POINT('Origin',(-7.105427357601E-14,49.5625000013656,-6.0924204042587E-14));
#5188=CARTESIAN_POINT('',(104.958734125,34.1875000013656,-6.0924204042587E-14));
#5189=CARTESIAN_POINT('',(104.958734125,33.9375000013656,-6.0924204042587E-14));
#5190=CARTESIAN_POINT('',(104.958734125,49.5625000013656,-1.089946703063E-13));
#5191=CARTESIAN_POINT('Ctrl Pts',(104.958734125,33.9375000013656,-1.28537377788739E-14));
#5192=CARTESIAN_POINT('Ctrl Pts',(104.958734125,33.8750000013656,43.4753311640868));
#5193=CARTESIAN_POINT('Ctrl Pts',(74.2170326445434,33.8125000013656,74.2170326445434));
#5194=CARTESIAN_POINT('Ctrl Pts',(43.4753311640869,33.7500000013656,104.958734125));
#5195=CARTESIAN_POINT('Ctrl Pts',(1.92806066683109E-14,33.6875000013656,
104.958734125));
#5196=CARTESIAN_POINT('Ctrl Pts',(-43.4753311640868,33.6250000013656,104.958734125));
#5197=CARTESIAN_POINT('Ctrl Pts',(-74.2170326445434,33.5625000013656,74.2170326445434));
#5198=CARTESIAN_POINT('Ctrl Pts',(-104.958734125,33.5000000013656,43.4753311640869));
#5199=CARTESIAN_POINT('Ctrl Pts',(-104.958734125,33.4375000013656,0.));
#5200=CARTESIAN_POINT('Ctrl Pts',(-104.958734125,33.3750000013656,-43.4753311640868));
#5201=CARTESIAN_POINT('Ctrl Pts',(-74.2170326445434,33.3125000013656,-74.2170326445434));
#5202=CARTESIAN_POINT('Ctrl Pts',(-43.4753311640868,33.2500000013656,-104.958734125));
#5203=CARTESIAN_POINT('Ctrl Pts',(-6.42686888943697E-15,33.1875000013656,
-104.958734125));
#5204=CARTESIAN_POINT('Ctrl Pts',(43.4753311640868,33.1250000013656,-104.958734125));
#5205=CARTESIAN_POINT('Ctrl Pts',(74.2170326445434,33.0625000013656,-74.2170326445434));
#5206=CARTESIAN_POINT('Ctrl Pts',(104.958734125,33.0000000013656,-43.4753311640868));
#5207=CARTESIAN_POINT('Ctrl Pts',(104.958734125,32.9375000013656,-1.28537377788739E-14));
#5208=CARTESIAN_POINT('Ctrl Pts',(104.958734125,34.1875000013656,-1.28537377788739E-14));
#5209=CARTESIAN_POINT('Ctrl Pts',(104.958734125,34.1250000013656,43.4753311640868));
#5210=CARTESIAN_POINT('Ctrl Pts',(74.2170326445434,34.0625000013656,74.2170326445434));
#5211=CARTESIAN_POINT('Ctrl Pts',(43.4753311640869,34.0000000013656,104.958734125));
#5212=CARTESIAN_POINT('Ctrl Pts',(1.92806066683109E-14,33.9375000013656,
104.958734125));
#5213=CARTESIAN_POINT('Ctrl Pts',(-43.4753311640868,33.8750000013656,104.958734125));
#5214=CARTESIAN_POINT('Ctrl Pts',(-74.2170326445434,33.8125000013656,74.2170326445434));
#5215=CARTESIAN_POINT('Ctrl Pts',(-104.958734125,33.7500000013656,43.4753311640869));
#5216=CARTESIAN_POINT('Ctrl Pts',(-104.958734125,33.6875000013656,0.));
#5217=CARTESIAN_POINT('Ctrl Pts',(-104.958734125,33.6250000013656,-43.4753311640868));
#5218=CARTESIAN_POINT('Ctrl Pts',(-74.2170326445434,33.5625000013656,-74.2170326445434));
#5219=CARTESIAN_POINT('Ctrl Pts',(-43.4753311640868,33.5000000013656,-104.958734125));
#5220=CARTESIAN_POINT('Ctrl Pts',(-6.42686888943697E-15,33.4375000013656,
-104.958734125));
#5221=CARTESIAN_POINT('Ctrl Pts',(43.4753311640868,33.3750000013656,-104.958734125));
#5222=CARTESIAN_POINT('Ctrl Pts',(74.2170326445434,33.3125000013656,-74.2170326445434));
#5223=CARTESIAN_POINT('Ctrl Pts',(104.958734125,33.2500000013656,-43.4753311640868));
#5224=CARTESIAN_POINT('Ctrl Pts',(104.958734125,33.1875000013656,-1.28537377788739E-14));
#5225=CARTESIAN_POINT('Origin',(-7.105427357601E-14,49.5625000013656,-6.0924204042587E-14));
#5226=CARTESIAN_POINT('',(104.958734125,35.1875000013656,-6.0924204042587E-14));
#5227=CARTESIAN_POINT('',(104.958734125,34.9375000013656,-6.0924204042587E-14));
#5228=CARTESIAN_POINT('',(104.958734125,49.5625000013656,-1.089946703063E-13));
#5229=CARTESIAN_POINT('Ctrl Pts',(104.958734125,34.9375000013656,-1.28537377788739E-14));
#5230=CARTESIAN_POINT('Ctrl Pts',(104.958734125,34.8750000013656,43.4753311640868));
#5231=CARTESIAN_POINT('Ctrl Pts',(74.2170326445434,34.8125000013656,74.2170326445434));
#5232=CARTESIAN_POINT('Ctrl Pts',(43.4753311640869,34.7500000013656,104.958734125));
#5233=CARTESIAN_POINT('Ctrl Pts',(1.92806066683109E-14,34.6875000013656,
104.958734125));
#5234=CARTESIAN_POINT('Ctrl Pts',(-43.4753311640868,34.6250000013656,104.958734125));
#5235=CARTESIAN_POINT('Ctrl Pts',(-74.2170326445434,34.5625000013656,74.2170326445434));
#5236=CARTESIAN_POINT('Ctrl Pts',(-104.958734125,34.5000000013656,43.4753311640869));
#5237=CARTESIAN_POINT('Ctrl Pts',(-104.958734125,34.4375000013656,0.));
#5238=CARTESIAN_POINT('Ctrl Pts',(-104.958734125,34.3750000013656,-43.4753311640868));
#5239=CARTESIAN_POINT('Ctrl Pts',(-74.2170326445434,34.3125000013656,-74.2170326445434));
#5240=CARTESIAN_POINT('Ctrl Pts',(-43.4753311640868,34.2500000013656,-104.958734125));
#5241=CARTESIAN_POINT('Ctrl Pts',(-6.42686888943697E-15,34.1875000013656,
-104.958734125));
#5242=CARTESIAN_POINT('Ctrl Pts',(43.4753311640868,34.1250000013656,-104.958734125));
#5243=CARTESIAN_POINT('Ctrl Pts',(74.2170326445434,34.0625000013656,-74.2170326445434));
#5244=CARTESIAN_POINT('Ctrl Pts',(104.958734125,34.0000000013656,-43.4753311640868));
#5245=CARTESIAN_POINT('Ctrl Pts',(104.958734125,33.9375000013656,-1.28537377788739E-14));
#5246=CARTESIAN_POINT('Ctrl Pts',(104.958734125,35.1875000013656,-1.28537377788739E-14));
#5247=CARTESIAN_POINT('Ctrl Pts',(104.958734125,35.1250000013656,43.4753311640868));
#5248=CARTESIAN_POINT('Ctrl Pts',(74.2170326445434,35.0625000013656,74.2170326445434));
#5249=CARTESIAN_POINT('Ctrl Pts',(43.4753311640869,35.0000000013656,104.958734125));
#5250=CARTESIAN_POINT('Ctrl Pts',(1.92806066683109E-14,34.9375000013656,
104.958734125));
#5251=CARTESIAN_POINT('Ctrl Pts',(-43.4753311640868,34.8750000013656,104.958734125));
#5252=CARTESIAN_POINT('Ctrl Pts',(-74.2170326445434,34.8125000013656,74.2170326445434));
#5253=CARTESIAN_POINT('Ctrl Pts',(-104.958734125,34.7500000013656,43.4753311640869));
#5254=CARTESIAN_POINT('Ctrl Pts',(-104.958734125,34.6875000013656,0.));
#5255=CARTESIAN_POINT('Ctrl Pts',(-104.958734125,34.6250000013656,-43.4753311640868));
#5256=CARTESIAN_POINT('Ctrl Pts',(-74.2170326445434,34.5625000013656,-74.2170326445434));
#5257=CARTESIAN_POINT('Ctrl Pts',(-43.4753311640868,34.5000000013656,-104.958734125));
#5258=CARTESIAN_POINT('Ctrl Pts',(-6.42686888943697E-15,34.4375000013656,
-104.958734125));
#5259=CARTESIAN_POINT('Ctrl Pts',(43.4753311640868,34.3750000013656,-104.958734125));
#5260=CARTESIAN_POINT('Ctrl Pts',(74.2170326445434,34.3125000013656,-74.2170326445434));
#5261=CARTESIAN_POINT('Ctrl Pts',(104.958734125,34.2500000013656,-43.4753311640868));
#5262=CARTESIAN_POINT('Ctrl Pts',(104.958734125,34.1875000013656,-1.28537377788739E-14));
#5263=CARTESIAN_POINT('Origin',(-7.105427357601E-14,49.5625000013656,-6.0924204042587E-14));
#5264=CARTESIAN_POINT('',(104.958734125,36.1875000013656,-6.0924204042587E-14));
#5265=CARTESIAN_POINT('',(104.958734125,35.9375000013656,-6.0924204042587E-14));
#5266=CARTESIAN_POINT('',(104.958734125,49.5625000013656,-1.089946703063E-13));
#5267=CARTESIAN_POINT('Ctrl Pts',(104.958734125,35.9375000013656,-1.28537377788739E-14));
#5268=CARTESIAN_POINT('Ctrl Pts',(104.958734125,35.8750000013656,43.4753311640868));
#5269=CARTESIAN_POINT('Ctrl Pts',(74.2170326445434,35.8125000013656,74.2170326445434));
#5270=CARTESIAN_POINT('Ctrl Pts',(43.4753311640869,35.7500000013656,104.958734125));
#5271=CARTESIAN_POINT('Ctrl Pts',(1.92806066683109E-14,35.6875000013656,
104.958734125));
#5272=CARTESIAN_POINT('Ctrl Pts',(-43.4753311640868,35.6250000013656,104.958734125));
#5273=CARTESIAN_POINT('Ctrl Pts',(-74.2170326445434,35.5625000013656,74.2170326445434));
#5274=CARTESIAN_POINT('Ctrl Pts',(-104.958734125,35.5000000013656,43.4753311640869));
#5275=CARTESIAN_POINT('Ctrl Pts',(-104.958734125,35.4375000013656,0.));
#5276=CARTESIAN_POINT('Ctrl Pts',(-104.958734125,35.3750000013656,-43.4753311640868));
#5277=CARTESIAN_POINT('Ctrl Pts',(-74.2170326445434,35.3125000013656,-74.2170326445434));
#5278=CARTESIAN_POINT('Ctrl Pts',(-43.4753311640868,35.2500000013656,-104.958734125));
#5279=CARTESIAN_POINT('Ctrl Pts',(-6.42686888943697E-15,35.1875000013656,
-104.958734125));
#5280=CARTESIAN_POINT('Ctrl Pts',(43.4753311640868,35.1250000013656,-104.958734125));
#5281=CARTESIAN_POINT('Ctrl Pts',(74.2170326445434,35.0625000013656,-74.2170326445434));
#5282=CARTESIAN_POINT('Ctrl Pts',(104.958734125,35.0000000013656,-43.4753311640868));
#5283=CARTESIAN_POINT('Ctrl Pts',(104.958734125,34.9375000013656,-1.28537377788739E-14));
#5284=CARTESIAN_POINT('Ctrl Pts',(104.958734125,36.1875000013656,-1.28537377788739E-14));
#5285=CARTESIAN_POINT('Ctrl Pts',(104.958734125,36.1250000013656,43.4753311640868));
#5286=CARTESIAN_POINT('Ctrl Pts',(74.2170326445434,36.0625000013656,74.2170326445434));
#5287=CARTESIAN_POINT('Ctrl Pts',(43.4753311640869,36.0000000013656,104.958734125));
#5288=CARTESIAN_POINT('Ctrl Pts',(1.92806066683109E-14,35.9375000013656,
104.958734125));
#5289=CARTESIAN_POINT('Ctrl Pts',(-43.4753311640868,35.8750000013656,104.958734125));
#5290=CARTESIAN_POINT('Ctrl Pts',(-74.2170326445434,35.8125000013656,74.2170326445434));
#5291=CARTESIAN_POINT('Ctrl Pts',(-104.958734125,35.7500000013656,43.4753311640869));
#5292=CARTESIAN_POINT('Ctrl Pts',(-104.958734125,35.6875000013656,0.));
#5293=CARTESIAN_POINT('Ctrl Pts',(-104.958734125,35.6250000013656,-43.4753311640868));
#5294=CARTESIAN_POINT('Ctrl Pts',(-74.2170326445434,35.5625000013656,-74.2170326445434));
#5295=CARTESIAN_POINT('Ctrl Pts',(-43.4753311640868,35.5000000013656,-104.958734125));
#5296=CARTESIAN_POINT('Ctrl Pts',(-6.42686888943697E-15,35.4375000013656,
-104.958734125));
#5297=CARTESIAN_POINT('Ctrl Pts',(43.4753311640868,35.3750000013656,-104.958734125));
#5298=CARTESIAN_POINT('Ctrl Pts',(74.2170326445434,35.3125000013656,-74.2170326445434));
#5299=CARTESIAN_POINT('Ctrl Pts',(104.958734125,35.2500000013656,-43.4753311640868));
#5300=CARTESIAN_POINT('Ctrl Pts',(104.958734125,35.1875000013656,-1.28537377788739E-14));
#5301=CARTESIAN_POINT('Origin',(-7.105427357601E-14,49.5625000013656,-6.0924204042587E-14));
#5302=CARTESIAN_POINT('',(104.958734125,37.1875000013656,-6.0924204042587E-14));
#5303=CARTESIAN_POINT('',(104.958734125,36.9375000013656,-6.0924204042587E-14));
#5304=CARTESIAN_POINT('',(104.958734125,49.5625000013656,-1.089946703063E-13));
#5305=CARTESIAN_POINT('Ctrl Pts',(104.958734125,36.9375000013656,-1.28537377788739E-14));
#5306=CARTESIAN_POINT('Ctrl Pts',(104.958734125,36.8750000013656,43.4753311640868));
#5307=CARTESIAN_POINT('Ctrl Pts',(74.2170326445434,36.8125000013656,74.2170326445434));
#5308=CARTESIAN_POINT('Ctrl Pts',(43.4753311640869,36.7500000013656,104.958734125));
#5309=CARTESIAN_POINT('Ctrl Pts',(1.92806066683109E-14,36.6875000013656,
104.958734125));
#5310=CARTESIAN_POINT('Ctrl Pts',(-43.4753311640868,36.6250000013656,104.958734125));
#5311=CARTESIAN_POINT('Ctrl Pts',(-74.2170326445434,36.5625000013656,74.2170326445434));
#5312=CARTESIAN_POINT('Ctrl Pts',(-104.958734125,36.5000000013656,43.4753311640869));
#5313=CARTESIAN_POINT('Ctrl Pts',(-104.958734125,36.4375000013656,0.));
#5314=CARTESIAN_POINT('Ctrl Pts',(-104.958734125,36.3750000013656,-43.4753311640868));
#5315=CARTESIAN_POINT('Ctrl Pts',(-74.2170326445434,36.3125000013656,-74.2170326445434));
#5316=CARTESIAN_POINT('Ctrl Pts',(-43.4753311640868,36.2500000013656,-104.958734125));
#5317=CARTESIAN_POINT('Ctrl Pts',(-6.42686888943697E-15,36.1875000013656,
-104.958734125));
#5318=CARTESIAN_POINT('Ctrl Pts',(43.4753311640868,36.1250000013656,-104.958734125));
#5319=CARTESIAN_POINT('Ctrl Pts',(74.2170326445434,36.0625000013656,-74.2170326445434));
#5320=CARTESIAN_POINT('Ctrl Pts',(104.958734125,36.0000000013656,-43.4753311640868));
#5321=CARTESIAN_POINT('Ctrl Pts',(104.958734125,35.9375000013656,-1.28537377788739E-14));
#5322=CARTESIAN_POINT('Ctrl Pts',(104.958734125,37.1875000013656,-1.28537377788739E-14));
#5323=CARTESIAN_POINT('Ctrl Pts',(104.958734125,37.1250000013656,43.4753311640868));
#5324=CARTESIAN_POINT('Ctrl Pts',(74.2170326445434,37.0625000013656,74.2170326445434));
#5325=CARTESIAN_POINT('Ctrl Pts',(43.4753311640869,37.0000000013656,104.958734125));
#5326=CARTESIAN_POINT('Ctrl Pts',(1.92806066683109E-14,36.9375000013656,
104.958734125));
#5327=CARTESIAN_POINT('Ctrl Pts',(-43.4753311640868,36.8750000013656,104.958734125));
#5328=CARTESIAN_POINT('Ctrl Pts',(-74.2170326445434,36.8125000013656,74.2170326445434));
#5329=CARTESIAN_POINT('Ctrl Pts',(-104.958734125,36.7500000013656,43.4753311640869));
#5330=CARTESIAN_POINT('Ctrl Pts',(-104.958734125,36.6875000013656,0.));
#5331=CARTESIAN_POINT('Ctrl Pts',(-104.958734125,36.6250000013656,-43.4753311640868));
#5332=CARTESIAN_POINT('Ctrl Pts',(-74.2170326445434,36.5625000013656,-74.2170326445434));
#5333=CARTESIAN_POINT('Ctrl Pts',(-43.4753311640868,36.5000000013656,-104.958734125));
#5334=CARTESIAN_POINT('Ctrl Pts',(-6.42686888943697E-15,36.4375000013656,
-104.958734125));
#5335=CARTESIAN_POINT('Ctrl Pts',(43.4753311640868,36.3750000013656,-104.958734125));
#5336=CARTESIAN_POINT('Ctrl Pts',(74.2170326445434,36.3125000013656,-74.2170326445434));
#5337=CARTESIAN_POINT('Ctrl Pts',(104.958734125,36.2500000013656,-43.4753311640868));
#5338=CARTESIAN_POINT('Ctrl Pts',(104.958734125,36.1875000013656,-1.28537377788739E-14));
#5339=CARTESIAN_POINT('Origin',(-7.105427357601E-14,49.5625000013656,-6.0924204042587E-14));
#5340=CARTESIAN_POINT('',(104.958734125,38.1875000013656,-6.0924204042587E-14));
#5341=CARTESIAN_POINT('',(104.958734125,37.9375000013656,-6.0924204042587E-14));
#5342=CARTESIAN_POINT('',(104.958734125,49.5625000013656,-1.089946703063E-13));
#5343=CARTESIAN_POINT('Ctrl Pts',(104.958734125,37.9375000013656,-1.28537377788739E-14));
#5344=CARTESIAN_POINT('Ctrl Pts',(104.958734125,37.8750000013656,43.4753311640868));
#5345=CARTESIAN_POINT('Ctrl Pts',(74.2170326445434,37.8125000013656,74.2170326445434));
#5346=CARTESIAN_POINT('Ctrl Pts',(43.4753311640869,37.7500000013656,104.958734125));
#5347=CARTESIAN_POINT('Ctrl Pts',(1.92806066683109E-14,37.6875000013656,
104.958734125));
#5348=CARTESIAN_POINT('Ctrl Pts',(-43.4753311640868,37.6250000013656,104.958734125));
#5349=CARTESIAN_POINT('Ctrl Pts',(-74.2170326445434,37.5625000013656,74.2170326445434));
#5350=CARTESIAN_POINT('Ctrl Pts',(-104.958734125,37.5000000013656,43.4753311640869));
#5351=CARTESIAN_POINT('Ctrl Pts',(-104.958734125,37.4375000013656,0.));
#5352=CARTESIAN_POINT('Ctrl Pts',(-104.958734125,37.3750000013656,-43.4753311640868));
#5353=CARTESIAN_POINT('Ctrl Pts',(-74.2170326445434,37.3125000013656,-74.2170326445434));
#5354=CARTESIAN_POINT('Ctrl Pts',(-43.4753311640868,37.2500000013656,-104.958734125));
#5355=CARTESIAN_POINT('Ctrl Pts',(-6.42686888943697E-15,37.1875000013656,
-104.958734125));
#5356=CARTESIAN_POINT('Ctrl Pts',(43.4753311640868,37.1250000013656,-104.958734125));
#5357=CARTESIAN_POINT('Ctrl Pts',(74.2170326445434,37.0625000013656,-74.2170326445434));
#5358=CARTESIAN_POINT('Ctrl Pts',(104.958734125,37.0000000013656,-43.4753311640868));
#5359=CARTESIAN_POINT('Ctrl Pts',(104.958734125,36.9375000013656,-1.28537377788739E-14));
#5360=CARTESIAN_POINT('Ctrl Pts',(104.958734125,38.1875000013656,-1.28537377788739E-14));
#5361=CARTESIAN_POINT('Ctrl Pts',(104.958734125,38.1250000013656,43.4753311640868));
#5362=CARTESIAN_POINT('Ctrl Pts',(74.2170326445434,38.0625000013656,74.2170326445434));
#5363=CARTESIAN_POINT('Ctrl Pts',(43.4753311640869,38.0000000013656,104.958734125));
#5364=CARTESIAN_POINT('Ctrl Pts',(1.92806066683109E-14,37.9375000013656,
104.958734125));
#5365=CARTESIAN_POINT('Ctrl Pts',(-43.4753311640868,37.8750000013656,104.958734125));
#5366=CARTESIAN_POINT('Ctrl Pts',(-74.2170326445434,37.8125000013656,74.2170326445434));
#5367=CARTESIAN_POINT('Ctrl Pts',(-104.958734125,37.7500000013656,43.4753311640869));
#5368=CARTESIAN_POINT('Ctrl Pts',(-104.958734125,37.6875000013656,0.));
#5369=CARTESIAN_POINT('Ctrl Pts',(-104.958734125,37.6250000013656,-43.4753311640868));
#5370=CARTESIAN_POINT('Ctrl Pts',(-74.2170326445434,37.5625000013656,-74.2170326445434));
#5371=CARTESIAN_POINT('Ctrl Pts',(-43.4753311640868,37.5000000013656,-104.958734125));
#5372=CARTESIAN_POINT('Ctrl Pts',(-6.42686888943697E-15,37.4375000013656,
-104.958734125));
#5373=CARTESIAN_POINT('Ctrl Pts',(43.4753311640868,37.3750000013656,-104.958734125));
#5374=CARTESIAN_POINT('Ctrl Pts',(74.2170326445434,37.3125000013656,-74.2170326445434));
#5375=CARTESIAN_POINT('Ctrl Pts',(104.958734125,37.2500000013656,-43.4753311640868));
#5376=CARTESIAN_POINT('Ctrl Pts',(104.958734125,37.1875000013656,-1.28537377788739E-14));
#5377=CARTESIAN_POINT('Origin',(-7.105427357601E-14,49.5625000013656,-6.0924204042587E-14));
#5378=CARTESIAN_POINT('',(104.958734125,39.1875000013656,-6.0924204042587E-14));
#5379=CARTESIAN_POINT('',(104.958734125,38.9375000013656,-6.0924204042587E-14));
#5380=CARTESIAN_POINT('',(104.958734125,49.5625000013656,-1.089946703063E-13));
#5381=CARTESIAN_POINT('Ctrl Pts',(104.958734125,38.9375000013656,-1.28537377788739E-14));
#5382=CARTESIAN_POINT('Ctrl Pts',(104.958734125,38.8750000013656,43.4753311640868));
#5383=CARTESIAN_POINT('Ctrl Pts',(74.2170326445434,38.8125000013656,74.2170326445434));
#5384=CARTESIAN_POINT('Ctrl Pts',(43.4753311640869,38.7500000013656,104.958734125));
#5385=CARTESIAN_POINT('Ctrl Pts',(1.92806066683109E-14,38.6875000013656,
104.958734125));
#5386=CARTESIAN_POINT('Ctrl Pts',(-43.4753311640868,38.6250000013656,104.958734125));
#5387=CARTESIAN_POINT('Ctrl Pts',(-74.2170326445434,38.5625000013656,74.2170326445434));
#5388=CARTESIAN_POINT('Ctrl Pts',(-104.958734125,38.5000000013656,43.4753311640869));
#5389=CARTESIAN_POINT('Ctrl Pts',(-104.958734125,38.4375000013656,0.));
#5390=CARTESIAN_POINT('Ctrl Pts',(-104.958734125,38.3750000013656,-43.4753311640868));
#5391=CARTESIAN_POINT('Ctrl Pts',(-74.2170326445434,38.3125000013656,-74.2170326445434));
#5392=CARTESIAN_POINT('Ctrl Pts',(-43.4753311640868,38.2500000013656,-104.958734125));
#5393=CARTESIAN_POINT('Ctrl Pts',(-6.42686888943697E-15,38.1875000013656,
-104.958734125));
#5394=CARTESIAN_POINT('Ctrl Pts',(43.4753311640868,38.1250000013656,-104.958734125));
#5395=CARTESIAN_POINT('Ctrl Pts',(74.2170326445434,38.0625000013656,-74.2170326445434));
#5396=CARTESIAN_POINT('Ctrl Pts',(104.958734125,38.0000000013656,-43.4753311640868));
#5397=CARTESIAN_POINT('Ctrl Pts',(104.958734125,37.9375000013656,-1.28537377788739E-14));
#5398=CARTESIAN_POINT('Ctrl Pts',(104.958734125,39.1875000013656,-1.28537377788739E-14));
#5399=CARTESIAN_POINT('Ctrl Pts',(104.958734125,39.1250000013656,43.4753311640868));
#5400=CARTESIAN_POINT('Ctrl Pts',(74.2170326445434,39.0625000013656,74.2170326445434));
#5401=CARTESIAN_POINT('Ctrl Pts',(43.4753311640869,39.0000000013656,104.958734125));
#5402=CARTESIAN_POINT('Ctrl Pts',(1.92806066683109E-14,38.9375000013656,
104.958734125));
#5403=CARTESIAN_POINT('Ctrl Pts',(-43.4753311640868,38.8750000013656,104.958734125));
#5404=CARTESIAN_POINT('Ctrl Pts',(-74.2170326445434,38.8125000013656,74.2170326445434));
#5405=CARTESIAN_POINT('Ctrl Pts',(-104.958734125,38.7500000013656,43.4753311640869));
#5406=CARTESIAN_POINT('Ctrl Pts',(-104.958734125,38.6875000013656,0.));
#5407=CARTESIAN_POINT('Ctrl Pts',(-104.958734125,38.6250000013656,-43.4753311640868));
#5408=CARTESIAN_POINT('Ctrl Pts',(-74.2170326445434,38.5625000013656,-74.2170326445434));
#5409=CARTESIAN_POINT('Ctrl Pts',(-43.4753311640868,38.5000000013656,-104.958734125));
#5410=CARTESIAN_POINT('Ctrl Pts',(-6.42686888943697E-15,38.4375000013656,
-104.958734125));
#5411=CARTESIAN_POINT('Ctrl Pts',(43.4753311640868,38.3750000013656,-104.958734125));
#5412=CARTESIAN_POINT('Ctrl Pts',(74.2170326445434,38.3125000013656,-74.2170326445434));
#5413=CARTESIAN_POINT('Ctrl Pts',(104.958734125,38.2500000013656,-43.4753311640868));
#5414=CARTESIAN_POINT('Ctrl Pts',(104.958734125,38.1875000013656,-1.28537377788739E-14));
#5415=CARTESIAN_POINT('Origin',(-7.105427357601E-14,49.5625000013656,-6.0924204042587E-14));
#5416=CARTESIAN_POINT('',(104.958734125,40.1875000013656,-6.0924204042587E-14));
#5417=CARTESIAN_POINT('',(104.958734125,39.9375000013656,-6.0924204042587E-14));
#5418=CARTESIAN_POINT('',(104.958734125,49.5625000013656,-1.089946703063E-13));
#5419=CARTESIAN_POINT('Ctrl Pts',(104.958734125,39.9375000013656,-1.28537377788739E-14));
#5420=CARTESIAN_POINT('Ctrl Pts',(104.958734125,39.8750000013656,43.4753311640868));
#5421=CARTESIAN_POINT('Ctrl Pts',(74.2170326445434,39.8125000013656,74.2170326445434));
#5422=CARTESIAN_POINT('Ctrl Pts',(43.4753311640869,39.7500000013656,104.958734125));
#5423=CARTESIAN_POINT('Ctrl Pts',(1.92806066683109E-14,39.6875000013656,
104.958734125));
#5424=CARTESIAN_POINT('Ctrl Pts',(-43.4753311640868,39.6250000013656,104.958734125));
#5425=CARTESIAN_POINT('Ctrl Pts',(-74.2170326445434,39.5625000013656,74.2170326445434));
#5426=CARTESIAN_POINT('Ctrl Pts',(-104.958734125,39.5000000013656,43.4753311640869));
#5427=CARTESIAN_POINT('Ctrl Pts',(-104.958734125,39.4375000013656,0.));
#5428=CARTESIAN_POINT('Ctrl Pts',(-104.958734125,39.3750000013656,-43.4753311640868));
#5429=CARTESIAN_POINT('Ctrl Pts',(-74.2170326445434,39.3125000013656,-74.2170326445434));
#5430=CARTESIAN_POINT('Ctrl Pts',(-43.4753311640868,39.2500000013656,-104.958734125));
#5431=CARTESIAN_POINT('Ctrl Pts',(-6.42686888943697E-15,39.1875000013656,
-104.958734125));
#5432=CARTESIAN_POINT('Ctrl Pts',(43.4753311640868,39.1250000013656,-104.958734125));
#5433=CARTESIAN_POINT('Ctrl Pts',(74.2170326445434,39.0625000013656,-74.2170326445434));
#5434=CARTESIAN_POINT('Ctrl Pts',(104.958734125,39.0000000013656,-43.4753311640868));
#5435=CARTESIAN_POINT('Ctrl Pts',(104.958734125,38.9375000013656,-1.28537377788739E-14));
#5436=CARTESIAN_POINT('Ctrl Pts',(104.958734125,40.1875000013656,-1.28537377788739E-14));
#5437=CARTESIAN_POINT('Ctrl Pts',(104.958734125,40.1250000013656,43.4753311640868));
#5438=CARTESIAN_POINT('Ctrl Pts',(74.2170326445434,40.0625000013656,74.2170326445434));
#5439=CARTESIAN_POINT('Ctrl Pts',(43.4753311640869,40.0000000013656,104.958734125));
#5440=CARTESIAN_POINT('Ctrl Pts',(1.92806066683109E-14,39.9375000013656,
104.958734125));
#5441=CARTESIAN_POINT('Ctrl Pts',(-43.4753311640868,39.8750000013656,104.958734125));
#5442=CARTESIAN_POINT('Ctrl Pts',(-74.2170326445434,39.8125000013656,74.2170326445434));
#5443=CARTESIAN_POINT('Ctrl Pts',(-104.958734125,39.7500000013656,43.4753311640869));
#5444=CARTESIAN_POINT('Ctrl Pts',(-104.958734125,39.6875000013656,0.));
#5445=CARTESIAN_POINT('Ctrl Pts',(-104.958734125,39.6250000013656,-43.4753311640868));
#5446=CARTESIAN_POINT('Ctrl Pts',(-74.2170326445434,39.5625000013656,-74.2170326445434));
#5447=CARTESIAN_POINT('Ctrl Pts',(-43.4753311640868,39.5000000013656,-104.958734125));
#5448=CARTESIAN_POINT('Ctrl Pts',(-6.42686888943697E-15,39.4375000013656,
-104.958734125));
#5449=CARTESIAN_POINT('Ctrl Pts',(43.4753311640868,39.3750000013656,-104.958734125));
#5450=CARTESIAN_POINT('Ctrl Pts',(74.2170326445434,39.3125000013656,-74.2170326445434));
#5451=CARTESIAN_POINT('Ctrl Pts',(104.958734125,39.2500000013656,-43.4753311640868));
#5452=CARTESIAN_POINT('Ctrl Pts',(104.958734125,39.1875000013656,-1.28537377788739E-14));
#5453=CARTESIAN_POINT('Origin',(-7.105427357601E-14,49.5625000013656,-6.0924204042587E-14));
#5454=CARTESIAN_POINT('',(104.958734125,41.1875000013656,-6.0924204042587E-14));
#5455=CARTESIAN_POINT('',(104.958734125,40.9375000013656,-6.0924204042587E-14));
#5456=CARTESIAN_POINT('',(104.958734125,49.5625000013656,-1.089946703063E-13));
#5457=CARTESIAN_POINT('Ctrl Pts',(104.958734125,40.9375000013656,-1.28537377788739E-14));
#5458=CARTESIAN_POINT('Ctrl Pts',(104.958734125,40.8750000013656,43.4753311640868));
#5459=CARTESIAN_POINT('Ctrl Pts',(74.2170326445434,40.8125000013656,74.2170326445434));
#5460=CARTESIAN_POINT('Ctrl Pts',(43.4753311640869,40.7500000013656,104.958734125));
#5461=CARTESIAN_POINT('Ctrl Pts',(1.92806066683109E-14,40.6875000013656,
104.958734125));
#5462=CARTESIAN_POINT('Ctrl Pts',(-43.4753311640868,40.6250000013656,104.958734125));
#5463=CARTESIAN_POINT('Ctrl Pts',(-74.2170326445434,40.5625000013656,74.2170326445434));
#5464=CARTESIAN_POINT('Ctrl Pts',(-104.958734125,40.5000000013656,43.4753311640869));
#5465=CARTESIAN_POINT('Ctrl Pts',(-104.958734125,40.4375000013656,0.));
#5466=CARTESIAN_POINT('Ctrl Pts',(-104.958734125,40.3750000013656,-43.4753311640868));
#5467=CARTESIAN_POINT('Ctrl Pts',(-74.2170326445434,40.3125000013656,-74.2170326445434));
#5468=CARTESIAN_POINT('Ctrl Pts',(-43.4753311640868,40.2500000013656,-104.958734125));
#5469=CARTESIAN_POINT('Ctrl Pts',(-6.42686888943697E-15,40.1875000013656,
-104.958734125));
#5470=CARTESIAN_POINT('Ctrl Pts',(43.4753311640868,40.1250000013656,-104.958734125));
#5471=CARTESIAN_POINT('Ctrl Pts',(74.2170326445434,40.0625000013656,-74.2170326445434));
#5472=CARTESIAN_POINT('Ctrl Pts',(104.958734125,40.0000000013656,-43.4753311640868));
#5473=CARTESIAN_POINT('Ctrl Pts',(104.958734125,39.9375000013656,-1.28537377788739E-14));
#5474=CARTESIAN_POINT('Ctrl Pts',(104.958734125,41.1875000013656,-1.28537377788739E-14));
#5475=CARTESIAN_POINT('Ctrl Pts',(104.958734125,41.1250000013656,43.4753311640868));
#5476=CARTESIAN_POINT('Ctrl Pts',(74.2170326445434,41.0625000013656,74.2170326445434));
#5477=CARTESIAN_POINT('Ctrl Pts',(43.4753311640869,41.0000000013656,104.958734125));
#5478=CARTESIAN_POINT('Ctrl Pts',(1.92806066683109E-14,40.9375000013656,
104.958734125));
#5479=CARTESIAN_POINT('Ctrl Pts',(-43.4753311640868,40.8750000013656,104.958734125));
#5480=CARTESIAN_POINT('Ctrl Pts',(-74.2170326445434,40.8125000013656,74.2170326445434));
#5481=CARTESIAN_POINT('Ctrl Pts',(-104.958734125,40.7500000013656,43.4753311640869));
#5482=CARTESIAN_POINT('Ctrl Pts',(-104.958734125,40.6875000013656,0.));
#5483=CARTESIAN_POINT('Ctrl Pts',(-104.958734125,40.6250000013656,-43.4753311640868));
#5484=CARTESIAN_POINT('Ctrl Pts',(-74.2170326445434,40.5625000013656,-74.2170326445434));
#5485=CARTESIAN_POINT('Ctrl Pts',(-43.4753311640868,40.5000000013656,-104.958734125));
#5486=CARTESIAN_POINT('Ctrl Pts',(-6.42686888943697E-15,40.4375000013656,
-104.958734125));
#5487=CARTESIAN_POINT('Ctrl Pts',(43.4753311640868,40.3750000013656,-104.958734125));
#5488=CARTESIAN_POINT('Ctrl Pts',(74.2170326445434,40.3125000013656,-74.2170326445434));
#5489=CARTESIAN_POINT('Ctrl Pts',(104.958734125,40.2500000013656,-43.4753311640868));
#5490=CARTESIAN_POINT('Ctrl Pts',(104.958734125,40.1875000013656,-1.28537377788739E-14));
#5491=CARTESIAN_POINT('Origin',(-7.105427357601E-14,49.5625000013656,-6.0924204042587E-14));
#5492=CARTESIAN_POINT('',(104.958734125,42.1875000013656,-6.0924204042587E-14));
#5493=CARTESIAN_POINT('',(104.958734125,41.9375000013656,-6.0924204042587E-14));
#5494=CARTESIAN_POINT('',(104.958734125,49.5625000013656,-1.089946703063E-13));
#5495=CARTESIAN_POINT('Ctrl Pts',(104.958734125,41.9375000013656,-1.28537377788739E-14));
#5496=CARTESIAN_POINT('Ctrl Pts',(104.958734125,41.8750000013656,43.4753311640868));
#5497=CARTESIAN_POINT('Ctrl Pts',(74.2170326445434,41.8125000013656,74.2170326445434));
#5498=CARTESIAN_POINT('Ctrl Pts',(43.4753311640869,41.7500000013656,104.958734125));
#5499=CARTESIAN_POINT('Ctrl Pts',(1.92806066683109E-14,41.6875000013656,
104.958734125));
#5500=CARTESIAN_POINT('Ctrl Pts',(-43.4753311640868,41.6250000013656,104.958734125));
#5501=CARTESIAN_POINT('Ctrl Pts',(-74.2170326445434,41.5625000013656,74.2170326445434));
#5502=CARTESIAN_POINT('Ctrl Pts',(-104.958734125,41.5000000013656,43.4753311640869));
#5503=CARTESIAN_POINT('Ctrl Pts',(-104.958734125,41.4375000013656,0.));
#5504=CARTESIAN_POINT('Ctrl Pts',(-104.958734125,41.3750000013656,-43.4753311640868));
#5505=CARTESIAN_POINT('Ctrl Pts',(-74.2170326445434,41.3125000013656,-74.2170326445434));
#5506=CARTESIAN_POINT('Ctrl Pts',(-43.4753311640868,41.2500000013656,-104.958734125));
#5507=CARTESIAN_POINT('Ctrl Pts',(-6.42686888943697E-15,41.1875000013656,
-104.958734125));
#5508=CARTESIAN_POINT('Ctrl Pts',(43.4753311640868,41.1250000013656,-104.958734125));
#5509=CARTESIAN_POINT('Ctrl Pts',(74.2170326445434,41.0625000013656,-74.2170326445434));
#5510=CARTESIAN_POINT('Ctrl Pts',(104.958734125,41.0000000013656,-43.4753311640868));
#5511=CARTESIAN_POINT('Ctrl Pts',(104.958734125,40.9375000013656,-1.28537377788739E-14));
#5512=CARTESIAN_POINT('Ctrl Pts',(104.958734125,42.1875000013656,-1.28537377788739E-14));
#5513=CARTESIAN_POINT('Ctrl Pts',(104.958734125,42.1250000013656,43.4753311640868));
#5514=CARTESIAN_POINT('Ctrl Pts',(74.2170326445434,42.0625000013656,74.2170326445434));
#5515=CARTESIAN_POINT('Ctrl Pts',(43.4753311640869,42.0000000013656,104.958734125));
#5516=CARTESIAN_POINT('Ctrl Pts',(1.92806066683109E-14,41.9375000013656,
104.958734125));
#5517=CARTESIAN_POINT('Ctrl Pts',(-43.4753311640868,41.8750000013656,104.958734125));
#5518=CARTESIAN_POINT('Ctrl Pts',(-74.2170326445434,41.8125000013656,74.2170326445434));
#5519=CARTESIAN_POINT('Ctrl Pts',(-104.958734125,41.7500000013656,43.4753311640869));
#5520=CARTESIAN_POINT('Ctrl Pts',(-104.958734125,41.6875000013656,0.));
#5521=CARTESIAN_POINT('Ctrl Pts',(-104.958734125,41.6250000013656,-43.4753311640868));
#5522=CARTESIAN_POINT('Ctrl Pts',(-74.2170326445434,41.5625000013656,-74.2170326445434));
#5523=CARTESIAN_POINT('Ctrl Pts',(-43.4753311640868,41.5000000013656,-104.958734125));
#5524=CARTESIAN_POINT('Ctrl Pts',(-6.42686888943697E-15,41.4375000013656,
-104.958734125));
#5525=CARTESIAN_POINT('Ctrl Pts',(43.4753311640868,41.3750000013656,-104.958734125));
#5526=CARTESIAN_POINT('Ctrl Pts',(74.2170326445434,41.3125000013656,-74.2170326445434));
#5527=CARTESIAN_POINT('Ctrl Pts',(104.958734125,41.2500000013656,-43.4753311640868));
#5528=CARTESIAN_POINT('Ctrl Pts',(104.958734125,41.1875000013656,-1.28537377788739E-14));
#5529=CARTESIAN_POINT('Origin',(-7.105427357601E-14,49.5625000013656,-6.0924204042587E-14));
#5530=CARTESIAN_POINT('',(104.958734125,43.1875000013656,-6.0924204042587E-14));
#5531=CARTESIAN_POINT('',(104.958734125,42.9375000013656,-6.0924204042587E-14));
#5532=CARTESIAN_POINT('',(104.958734125,49.5625000013656,-1.089946703063E-13));
#5533=CARTESIAN_POINT('Ctrl Pts',(104.958734125,42.9375000013656,-1.28537377788739E-14));
#5534=CARTESIAN_POINT('Ctrl Pts',(104.958734125,42.8750000013656,43.4753311640868));
#5535=CARTESIAN_POINT('Ctrl Pts',(74.2170326445434,42.8125000013656,74.2170326445434));
#5536=CARTESIAN_POINT('Ctrl Pts',(43.4753311640869,42.7500000013656,104.958734125));
#5537=CARTESIAN_POINT('Ctrl Pts',(1.92806066683109E-14,42.6875000013656,
104.958734125));
#5538=CARTESIAN_POINT('Ctrl Pts',(-43.4753311640868,42.6250000013656,104.958734125));
#5539=CARTESIAN_POINT('Ctrl Pts',(-74.2170326445434,42.5625000013656,74.2170326445434));
#5540=CARTESIAN_POINT('Ctrl Pts',(-104.958734125,42.5000000013656,43.4753311640869));
#5541=CARTESIAN_POINT('Ctrl Pts',(-104.958734125,42.4375000013656,0.));
#5542=CARTESIAN_POINT('Ctrl Pts',(-104.958734125,42.3750000013656,-43.4753311640868));
#5543=CARTESIAN_POINT('Ctrl Pts',(-74.2170326445434,42.3125000013656,-74.2170326445434));
#5544=CARTESIAN_POINT('Ctrl Pts',(-43.4753311640868,42.2500000013656,-104.958734125));
#5545=CARTESIAN_POINT('Ctrl Pts',(-6.42686888943697E-15,42.1875000013656,
-104.958734125));
#5546=CARTESIAN_POINT('Ctrl Pts',(43.4753311640868,42.1250000013656,-104.958734125));
#5547=CARTESIAN_POINT('Ctrl Pts',(74.2170326445434,42.0625000013656,-74.2170326445434));
#5548=CARTESIAN_POINT('Ctrl Pts',(104.958734125,42.0000000013656,-43.4753311640868));
#5549=CARTESIAN_POINT('Ctrl Pts',(104.958734125,41.9375000013656,-1.28537377788739E-14));
#5550=CARTESIAN_POINT('Ctrl Pts',(104.958734125,43.1875000013656,-1.28537377788739E-14));
#5551=CARTESIAN_POINT('Ctrl Pts',(104.958734125,43.1250000013656,43.4753311640868));
#5552=CARTESIAN_POINT('Ctrl Pts',(74.2170326445434,43.0625000013656,74.2170326445434));
#5553=CARTESIAN_POINT('Ctrl Pts',(43.4753311640869,43.0000000013656,104.958734125));
#5554=CARTESIAN_POINT('Ctrl Pts',(1.92806066683109E-14,42.9375000013656,
104.958734125));
#5555=CARTESIAN_POINT('Ctrl Pts',(-43.4753311640868,42.8750000013656,104.958734125));
#5556=CARTESIAN_POINT('Ctrl Pts',(-74.2170326445434,42.8125000013656,74.2170326445434));
#5557=CARTESIAN_POINT('Ctrl Pts',(-104.958734125,42.7500000013656,43.4753311640869));
#5558=CARTESIAN_POINT('Ctrl Pts',(-104.958734125,42.6875000013656,0.));
#5559=CARTESIAN_POINT('Ctrl Pts',(-104.958734125,42.6250000013656,-43.4753311640868));
#5560=CARTESIAN_POINT('Ctrl Pts',(-74.2170326445434,42.5625000013656,-74.2170326445434));
#5561=CARTESIAN_POINT('Ctrl Pts',(-43.4753311640868,42.5000000013656,-104.958734125));
#5562=CARTESIAN_POINT('Ctrl Pts',(-6.42686888943697E-15,42.4375000013656,
-104.958734125));
#5563=CARTESIAN_POINT('Ctrl Pts',(43.4753311640868,42.3750000013656,-104.958734125));
#5564=CARTESIAN_POINT('Ctrl Pts',(74.2170326445434,42.3125000013656,-74.2170326445434));
#5565=CARTESIAN_POINT('Ctrl Pts',(104.958734125,42.2500000013656,-43.4753311640868));
#5566=CARTESIAN_POINT('Ctrl Pts',(104.958734125,42.1875000013656,-1.28537377788739E-14));
#5567=CARTESIAN_POINT('Origin',(-7.105427357601E-14,49.5625000013656,-6.0924204042587E-14));
#5568=CARTESIAN_POINT('',(104.958734125,44.1875000013656,-6.0924204042587E-14));
#5569=CARTESIAN_POINT('',(104.958734125,43.9375000013656,-6.0924204042587E-14));
#5570=CARTESIAN_POINT('',(104.958734125,49.5625000013656,-1.089946703063E-13));
#5571=CARTESIAN_POINT('Ctrl Pts',(104.958734125,43.9375000013656,-1.28537377788739E-14));
#5572=CARTESIAN_POINT('Ctrl Pts',(104.958734125,43.8750000013656,43.4753311640868));
#5573=CARTESIAN_POINT('Ctrl Pts',(74.2170326445434,43.8125000013656,74.2170326445434));
#5574=CARTESIAN_POINT('Ctrl Pts',(43.4753311640869,43.7500000013656,104.958734125));
#5575=CARTESIAN_POINT('Ctrl Pts',(1.92806066683109E-14,43.6875000013656,
104.958734125));
#5576=CARTESIAN_POINT('Ctrl Pts',(-43.4753311640868,43.6250000013656,104.958734125));
#5577=CARTESIAN_POINT('Ctrl Pts',(-74.2170326445434,43.5625000013656,74.2170326445434));
#5578=CARTESIAN_POINT('Ctrl Pts',(-104.958734125,43.5000000013656,43.4753311640869));
#5579=CARTESIAN_POINT('Ctrl Pts',(-104.958734125,43.4375000013656,0.));
#5580=CARTESIAN_POINT('Ctrl Pts',(-104.958734125,43.3750000013656,-43.4753311640868));
#5581=CARTESIAN_POINT('Ctrl Pts',(-74.2170326445434,43.3125000013656,-74.2170326445434));
#5582=CARTESIAN_POINT('Ctrl Pts',(-43.4753311640868,43.2500000013656,-104.958734125));
#5583=CARTESIAN_POINT('Ctrl Pts',(-6.42686888943697E-15,43.1875000013656,
-104.958734125));
#5584=CARTESIAN_POINT('Ctrl Pts',(43.4753311640868,43.1250000013656,-104.958734125));
#5585=CARTESIAN_POINT('Ctrl Pts',(74.2170326445434,43.0625000013656,-74.2170326445434));
#5586=CARTESIAN_POINT('Ctrl Pts',(104.958734125,43.0000000013656,-43.4753311640868));
#5587=CARTESIAN_POINT('Ctrl Pts',(104.958734125,42.9375000013656,-1.28537377788739E-14));
#5588=CARTESIAN_POINT('Ctrl Pts',(104.958734125,44.1875000013656,-1.28537377788739E-14));
#5589=CARTESIAN_POINT('Ctrl Pts',(104.958734125,44.1250000013656,43.4753311640868));
#5590=CARTESIAN_POINT('Ctrl Pts',(74.2170326445434,44.0625000013656,74.2170326445434));
#5591=CARTESIAN_POINT('Ctrl Pts',(43.4753311640869,44.0000000013656,104.958734125));
#5592=CARTESIAN_POINT('Ctrl Pts',(1.92806066683109E-14,43.9375000013656,
104.958734125));
#5593=CARTESIAN_POINT('Ctrl Pts',(-43.4753311640868,43.8750000013656,104.958734125));
#5594=CARTESIAN_POINT('Ctrl Pts',(-74.2170326445434,43.8125000013656,74.2170326445434));
#5595=CARTESIAN_POINT('Ctrl Pts',(-104.958734125,43.7500000013656,43.4753311640869));
#5596=CARTESIAN_POINT('Ctrl Pts',(-104.958734125,43.6875000013656,0.));
#5597=CARTESIAN_POINT('Ctrl Pts',(-104.958734125,43.6250000013656,-43.4753311640868));
#5598=CARTESIAN_POINT('Ctrl Pts',(-74.2170326445434,43.5625000013656,-74.2170326445434));
#5599=CARTESIAN_POINT('Ctrl Pts',(-43.4753311640868,43.5000000013656,-104.958734125));
#5600=CARTESIAN_POINT('Ctrl Pts',(-6.42686888943697E-15,43.4375000013656,
-104.958734125));
#5601=CARTESIAN_POINT('Ctrl Pts',(43.4753311640868,43.3750000013656,-104.958734125));
#5602=CARTESIAN_POINT('Ctrl Pts',(74.2170326445434,43.3125000013656,-74.2170326445434));
#5603=CARTESIAN_POINT('Ctrl Pts',(104.958734125,43.2500000013656,-43.4753311640868));
#5604=CARTESIAN_POINT('Ctrl Pts',(104.958734125,43.1875000013656,-1.28537377788739E-14));
#5605=CARTESIAN_POINT('Origin',(-7.105427357601E-14,49.5625000013656,-6.0924204042587E-14));
#5606=CARTESIAN_POINT('',(104.958734125,45.1875000013656,-6.0924204042587E-14));
#5607=CARTESIAN_POINT('',(104.958734125,44.9375000013656,-6.0924204042587E-14));
#5608=CARTESIAN_POINT('',(104.958734125,49.5625000013656,-1.089946703063E-13));
#5609=CARTESIAN_POINT('Ctrl Pts',(104.958734125,44.9375000013656,-1.28537377788739E-14));
#5610=CARTESIAN_POINT('Ctrl Pts',(104.958734125,44.8750000013656,43.4753311640868));
#5611=CARTESIAN_POINT('Ctrl Pts',(74.2170326445434,44.8125000013656,74.2170326445434));
#5612=CARTESIAN_POINT('Ctrl Pts',(43.4753311640869,44.7500000013656,104.958734125));
#5613=CARTESIAN_POINT('Ctrl Pts',(1.92806066683109E-14,44.6875000013656,
104.958734125));
#5614=CARTESIAN_POINT('Ctrl Pts',(-43.4753311640868,44.6250000013656,104.958734125));
#5615=CARTESIAN_POINT('Ctrl Pts',(-74.2170326445434,44.5625000013656,74.2170326445434));
#5616=CARTESIAN_POINT('Ctrl Pts',(-104.958734125,44.5000000013656,43.4753311640869));
#5617=CARTESIAN_POINT('Ctrl Pts',(-104.958734125,44.4375000013656,0.));
#5618=CARTESIAN_POINT('Ctrl Pts',(-104.958734125,44.3750000013656,-43.4753311640868));
#5619=CARTESIAN_POINT('Ctrl Pts',(-74.2170326445434,44.3125000013656,-74.2170326445434));
#5620=CARTESIAN_POINT('Ctrl Pts',(-43.4753311640868,44.2500000013656,-104.958734125));
#5621=CARTESIAN_POINT('Ctrl Pts',(-6.42686888943697E-15,44.1875000013656,
-104.958734125));
#5622=CARTESIAN_POINT('Ctrl Pts',(43.4753311640868,44.1250000013656,-104.958734125));
#5623=CARTESIAN_POINT('Ctrl Pts',(74.2170326445434,44.0625000013656,-74.2170326445434));
#5624=CARTESIAN_POINT('Ctrl Pts',(104.958734125,44.0000000013656,-43.4753311640868));
#5625=CARTESIAN_POINT('Ctrl Pts',(104.958734125,43.9375000013656,-1.28537377788739E-14));
#5626=CARTESIAN_POINT('Ctrl Pts',(104.958734125,45.1875000013656,-1.28537377788739E-14));
#5627=CARTESIAN_POINT('Ctrl Pts',(104.958734125,45.1250000013656,43.4753311640868));
#5628=CARTESIAN_POINT('Ctrl Pts',(74.2170326445434,45.0625000013656,74.2170326445434));
#5629=CARTESIAN_POINT('Ctrl Pts',(43.4753311640869,45.0000000013656,104.958734125));
#5630=CARTESIAN_POINT('Ctrl Pts',(1.92806066683109E-14,44.9375000013656,
104.958734125));
#5631=CARTESIAN_POINT('Ctrl Pts',(-43.4753311640868,44.8750000013656,104.958734125));
#5632=CARTESIAN_POINT('Ctrl Pts',(-74.2170326445434,44.8125000013656,74.2170326445434));
#5633=CARTESIAN_POINT('Ctrl Pts',(-104.958734125,44.7500000013656,43.4753311640869));
#5634=CARTESIAN_POINT('Ctrl Pts',(-104.958734125,44.6875000013656,0.));
#5635=CARTESIAN_POINT('Ctrl Pts',(-104.958734125,44.6250000013656,-43.4753311640868));
#5636=CARTESIAN_POINT('Ctrl Pts',(-74.2170326445434,44.5625000013656,-74.2170326445434));
#5637=CARTESIAN_POINT('Ctrl Pts',(-43.4753311640868,44.5000000013656,-104.958734125));
#5638=CARTESIAN_POINT('Ctrl Pts',(-6.42686888943697E-15,44.4375000013656,
-104.958734125));
#5639=CARTESIAN_POINT('Ctrl Pts',(43.4753311640868,44.3750000013656,-104.958734125));
#5640=CARTESIAN_POINT('Ctrl Pts',(74.2170326445434,44.3125000013656,-74.2170326445434));
#5641=CARTESIAN_POINT('Ctrl Pts',(104.958734125,44.2500000013656,-43.4753311640868));
#5642=CARTESIAN_POINT('Ctrl Pts',(104.958734125,44.1875000013656,-1.28537377788739E-14));
#5643=CARTESIAN_POINT('Origin',(-7.105427357601E-14,49.5625000013656,-6.0924204042587E-14));
#5644=CARTESIAN_POINT('',(104.958734125,46.1875000013656,-6.0924204042587E-14));
#5645=CARTESIAN_POINT('',(104.958734125,45.9375000013656,-6.0924204042587E-14));
#5646=CARTESIAN_POINT('',(104.958734125,49.5625000013656,-1.089946703063E-13));
#5647=CARTESIAN_POINT('Ctrl Pts',(104.958734125,45.9375000013656,-1.28537377788739E-14));
#5648=CARTESIAN_POINT('Ctrl Pts',(104.958734125,45.8750000013656,43.4753311640868));
#5649=CARTESIAN_POINT('Ctrl Pts',(74.2170326445434,45.8125000013656,74.2170326445434));
#5650=CARTESIAN_POINT('Ctrl Pts',(43.4753311640869,45.7500000013656,104.958734125));
#5651=CARTESIAN_POINT('Ctrl Pts',(1.92806066683109E-14,45.6875000013656,
104.958734125));
#5652=CARTESIAN_POINT('Ctrl Pts',(-43.4753311640868,45.6250000013656,104.958734125));
#5653=CARTESIAN_POINT('Ctrl Pts',(-74.2170326445434,45.5625000013656,74.2170326445434));
#5654=CARTESIAN_POINT('Ctrl Pts',(-104.958734125,45.5000000013656,43.4753311640869));
#5655=CARTESIAN_POINT('Ctrl Pts',(-104.958734125,45.4375000013656,0.));
#5656=CARTESIAN_POINT('Ctrl Pts',(-104.958734125,45.3750000013656,-43.4753311640868));
#5657=CARTESIAN_POINT('Ctrl Pts',(-74.2170326445434,45.3125000013656,-74.2170326445434));
#5658=CARTESIAN_POINT('Ctrl Pts',(-43.4753311640868,45.2500000013656,-104.958734125));
#5659=CARTESIAN_POINT('Ctrl Pts',(-6.42686888943697E-15,45.1875000013656,
-104.958734125));
#5660=CARTESIAN_POINT('Ctrl Pts',(43.4753311640868,45.1250000013656,-104.958734125));
#5661=CARTESIAN_POINT('Ctrl Pts',(74.2170326445434,45.0625000013656,-74.2170326445434));
#5662=CARTESIAN_POINT('Ctrl Pts',(104.958734125,45.0000000013656,-43.4753311640868));
#5663=CARTESIAN_POINT('Ctrl Pts',(104.958734125,44.9375000013656,-1.28537377788739E-14));
#5664=CARTESIAN_POINT('Ctrl Pts',(104.958734125,46.1875000013656,-1.28537377788739E-14));
#5665=CARTESIAN_POINT('Ctrl Pts',(104.958734125,46.1250000013656,43.4753311640868));
#5666=CARTESIAN_POINT('Ctrl Pts',(74.2170326445434,46.0625000013656,74.2170326445434));
#5667=CARTESIAN_POINT('Ctrl Pts',(43.4753311640869,46.0000000013656,104.958734125));
#5668=CARTESIAN_POINT('Ctrl Pts',(1.92806066683109E-14,45.9375000013656,
104.958734125));
#5669=CARTESIAN_POINT('Ctrl Pts',(-43.4753311640868,45.8750000013656,104.958734125));
#5670=CARTESIAN_POINT('Ctrl Pts',(-74.2170326445434,45.8125000013656,74.2170326445434));
#5671=CARTESIAN_POINT('Ctrl Pts',(-104.958734125,45.7500000013656,43.4753311640869));
#5672=CARTESIAN_POINT('Ctrl Pts',(-104.958734125,45.6875000013656,0.));
#5673=CARTESIAN_POINT('Ctrl Pts',(-104.958734125,45.6250000013656,-43.4753311640868));
#5674=CARTESIAN_POINT('Ctrl Pts',(-74.2170326445434,45.5625000013656,-74.2170326445434));
#5675=CARTESIAN_POINT('Ctrl Pts',(-43.4753311640868,45.5000000013656,-104.958734125));
#5676=CARTESIAN_POINT('Ctrl Pts',(-6.42686888943697E-15,45.4375000013656,
-104.958734125));
#5677=CARTESIAN_POINT('Ctrl Pts',(43.4753311640868,45.3750000013656,-104.958734125));
#5678=CARTESIAN_POINT('Ctrl Pts',(74.2170326445434,45.3125000013656,-74.2170326445434));
#5679=CARTESIAN_POINT('Ctrl Pts',(104.958734125,45.2500000013656,-43.4753311640868));
#5680=CARTESIAN_POINT('Ctrl Pts',(104.958734125,45.1875000013656,-1.28537377788739E-14));
#5681=CARTESIAN_POINT('Origin',(-7.105427357601E-14,49.5625000013656,-6.0924204042587E-14));
#5682=CARTESIAN_POINT('',(104.958734125,47.1875000013656,-6.0924204042587E-14));
#5683=CARTESIAN_POINT('',(104.958734125,46.9375000013656,-6.0924204042587E-14));
#5684=CARTESIAN_POINT('',(104.958734125,49.5625000013656,-1.089946703063E-13));
#5685=CARTESIAN_POINT('Ctrl Pts',(104.958734125,46.9375000013656,-1.28537377788739E-14));
#5686=CARTESIAN_POINT('Ctrl Pts',(104.958734125,46.8750000013656,43.4753311640868));
#5687=CARTESIAN_POINT('Ctrl Pts',(74.2170326445434,46.8125000013656,74.2170326445434));
#5688=CARTESIAN_POINT('Ctrl Pts',(43.4753311640869,46.7500000013656,104.958734125));
#5689=CARTESIAN_POINT('Ctrl Pts',(1.92806066683109E-14,46.6875000013656,
104.958734125));
#5690=CARTESIAN_POINT('Ctrl Pts',(-43.4753311640868,46.6250000013656,104.958734125));
#5691=CARTESIAN_POINT('Ctrl Pts',(-74.2170326445434,46.5625000013656,74.2170326445434));
#5692=CARTESIAN_POINT('Ctrl Pts',(-104.958734125,46.5000000013656,43.4753311640869));
#5693=CARTESIAN_POINT('Ctrl Pts',(-104.958734125,46.4375000013656,0.));
#5694=CARTESIAN_POINT('Ctrl Pts',(-104.958734125,46.3750000013656,-43.4753311640868));
#5695=CARTESIAN_POINT('Ctrl Pts',(-74.2170326445434,46.3125000013656,-74.2170326445434));
#5696=CARTESIAN_POINT('Ctrl Pts',(-43.4753311640868,46.2500000013656,-104.958734125));
#5697=CARTESIAN_POINT('Ctrl Pts',(-6.42686888943697E-15,46.1875000013656,
-104.958734125));
#5698=CARTESIAN_POINT('Ctrl Pts',(43.4753311640868,46.1250000013656,-104.958734125));
#5699=CARTESIAN_POINT('Ctrl Pts',(74.2170326445434,46.0625000013656,-74.2170326445434));
#5700=CARTESIAN_POINT('Ctrl Pts',(104.958734125,46.0000000013656,-43.4753311640868));
#5701=CARTESIAN_POINT('Ctrl Pts',(104.958734125,45.9375000013656,-1.28537377788739E-14));
#5702=CARTESIAN_POINT('Ctrl Pts',(104.958734125,47.1875000013656,-1.28537377788739E-14));
#5703=CARTESIAN_POINT('Ctrl Pts',(104.958734125,47.1250000013656,43.4753311640868));
#5704=CARTESIAN_POINT('Ctrl Pts',(74.2170326445434,47.0625000013656,74.2170326445434));
#5705=CARTESIAN_POINT('Ctrl Pts',(43.4753311640869,47.0000000013656,104.958734125));
#5706=CARTESIAN_POINT('Ctrl Pts',(1.92806066683109E-14,46.9375000013656,
104.958734125));
#5707=CARTESIAN_POINT('Ctrl Pts',(-43.4753311640868,46.8750000013656,104.958734125));
#5708=CARTESIAN_POINT('Ctrl Pts',(-74.2170326445434,46.8125000013656,74.2170326445434));
#5709=CARTESIAN_POINT('Ctrl Pts',(-104.958734125,46.7500000013656,43.4753311640869));
#5710=CARTESIAN_POINT('Ctrl Pts',(-104.958734125,46.6875000013656,0.));
#5711=CARTESIAN_POINT('Ctrl Pts',(-104.958734125,46.6250000013656,-43.4753311640868));
#5712=CARTESIAN_POINT('Ctrl Pts',(-74.2170326445434,46.5625000013656,-74.2170326445434));
#5713=CARTESIAN_POINT('Ctrl Pts',(-43.4753311640868,46.5000000013656,-104.958734125));
#5714=CARTESIAN_POINT('Ctrl Pts',(-6.42686888943697E-15,46.4375000013656,
-104.958734125));
#5715=CARTESIAN_POINT('Ctrl Pts',(43.4753311640868,46.3750000013656,-104.958734125));
#5716=CARTESIAN_POINT('Ctrl Pts',(74.2170326445434,46.3125000013656,-74.2170326445434));
#5717=CARTESIAN_POINT('Ctrl Pts',(104.958734125,46.2500000013656,-43.4753311640868));
#5718=CARTESIAN_POINT('Ctrl Pts',(104.958734125,46.1875000013656,-1.28537377788739E-14));
#5719=CARTESIAN_POINT('Origin',(-7.105427357601E-14,49.5625000013656,-6.0924204042587E-14));
#5720=CARTESIAN_POINT('',(104.958734125,48.1875000013656,-6.0924204042587E-14));
#5721=CARTESIAN_POINT('',(104.958734125,47.9375000013656,-6.0924204042587E-14));
#5722=CARTESIAN_POINT('',(104.958734125,49.5625000013656,-1.089946703063E-13));
#5723=CARTESIAN_POINT('Ctrl Pts',(104.958734125,47.9375000013656,-1.28537377788739E-14));
#5724=CARTESIAN_POINT('Ctrl Pts',(104.958734125,47.8750000013656,43.4753311640868));
#5725=CARTESIAN_POINT('Ctrl Pts',(74.2170326445434,47.8125000013656,74.2170326445434));
#5726=CARTESIAN_POINT('Ctrl Pts',(43.4753311640869,47.7500000013656,104.958734125));
#5727=CARTESIAN_POINT('Ctrl Pts',(1.92806066683109E-14,47.6875000013656,
104.958734125));
#5728=CARTESIAN_POINT('Ctrl Pts',(-43.4753311640868,47.6250000013656,104.958734125));
#5729=CARTESIAN_POINT('Ctrl Pts',(-74.2170326445434,47.5625000013656,74.2170326445434));
#5730=CARTESIAN_POINT('Ctrl Pts',(-104.958734125,47.5000000013656,43.4753311640869));
#5731=CARTESIAN_POINT('Ctrl Pts',(-104.958734125,47.4375000013656,0.));
#5732=CARTESIAN_POINT('Ctrl Pts',(-104.958734125,47.3750000013656,-43.4753311640868));
#5733=CARTESIAN_POINT('Ctrl Pts',(-74.2170326445434,47.3125000013656,-74.2170326445434));
#5734=CARTESIAN_POINT('Ctrl Pts',(-43.4753311640868,47.2500000013656,-104.958734125));
#5735=CARTESIAN_POINT('Ctrl Pts',(-6.42686888943697E-15,47.1875000013656,
-104.958734125));
#5736=CARTESIAN_POINT('Ctrl Pts',(43.4753311640868,47.1250000013656,-104.958734125));
#5737=CARTESIAN_POINT('Ctrl Pts',(74.2170326445434,47.0625000013656,-74.2170326445434));
#5738=CARTESIAN_POINT('Ctrl Pts',(104.958734125,47.0000000013656,-43.4753311640868));
#5739=CARTESIAN_POINT('Ctrl Pts',(104.958734125,46.9375000013656,-1.28537377788739E-14));
#5740=CARTESIAN_POINT('Ctrl Pts',(104.958734125,48.1875000013656,-1.28537377788739E-14));
#5741=CARTESIAN_POINT('Ctrl Pts',(104.958734125,48.1250000013656,43.4753311640868));
#5742=CARTESIAN_POINT('Ctrl Pts',(74.2170326445434,48.0625000013656,74.2170326445434));
#5743=CARTESIAN_POINT('Ctrl Pts',(43.4753311640869,48.0000000013656,104.958734125));
#5744=CARTESIAN_POINT('Ctrl Pts',(1.92806066683109E-14,47.9375000013656,
104.958734125));
#5745=CARTESIAN_POINT('Ctrl Pts',(-43.4753311640868,47.8750000013656,104.958734125));
#5746=CARTESIAN_POINT('Ctrl Pts',(-74.2170326445434,47.8125000013656,74.2170326445434));
#5747=CARTESIAN_POINT('Ctrl Pts',(-104.958734125,47.7500000013656,43.4753311640869));
#5748=CARTESIAN_POINT('Ctrl Pts',(-104.958734125,47.6875000013656,0.));
#5749=CARTESIAN_POINT('Ctrl Pts',(-104.958734125,47.6250000013656,-43.4753311640868));
#5750=CARTESIAN_POINT('Ctrl Pts',(-74.2170326445434,47.5625000013656,-74.2170326445434));
#5751=CARTESIAN_POINT('Ctrl Pts',(-43.4753311640868,47.5000000013656,-104.958734125));
#5752=CARTESIAN_POINT('Ctrl Pts',(-6.42686888943697E-15,47.4375000013656,
-104.958734125));
#5753=CARTESIAN_POINT('Ctrl Pts',(43.4753311640868,47.3750000013656,-104.958734125));
#5754=CARTESIAN_POINT('Ctrl Pts',(74.2170326445434,47.3125000013656,-74.2170326445434));
#5755=CARTESIAN_POINT('Ctrl Pts',(104.958734125,47.2500000013656,-43.4753311640868));
#5756=CARTESIAN_POINT('Ctrl Pts',(104.958734125,47.1875000013656,-1.28537377788739E-14));
#5757=CARTESIAN_POINT('Origin',(-7.105427357601E-14,49.5625000013656,-6.0924204042587E-14));
#5758=CARTESIAN_POINT('',(104.958734125,49.1875000013656,-6.0924204042587E-14));
#5759=CARTESIAN_POINT('',(104.958734125,48.9375000013656,-6.0924204042587E-14));
#5760=CARTESIAN_POINT('',(104.958734125,49.5625000013656,-1.089946703063E-13));
#5761=CARTESIAN_POINT('',(-104.958734125,49.6875000013656,0.));
#5762=CARTESIAN_POINT('Ctrl Pts',(-104.958734125,49.6875000013656,0.));
#5763=CARTESIAN_POINT('Ctrl Pts',(-104.958734125,49.6250000013656,-43.4753311640868));
#5764=CARTESIAN_POINT('Ctrl Pts',(-74.2170326445434,49.5625000013656,-74.2170326445434));
#5765=CARTESIAN_POINT('Ctrl Pts',(-43.4753311640868,49.5000000013656,-104.958734125));
#5766=CARTESIAN_POINT('Ctrl Pts',(-6.42686888943697E-15,49.4375000013656,
-104.958734125));
#5767=CARTESIAN_POINT('Ctrl Pts',(43.4753311640868,49.3750000013656,-104.958734125));
#5768=CARTESIAN_POINT('Ctrl Pts',(74.2170326445434,49.3125000013656,-74.2170326445434));
#5769=CARTESIAN_POINT('Ctrl Pts',(104.958734125,49.2500000013656,-43.4753311640868));
#5770=CARTESIAN_POINT('Ctrl Pts',(104.958734125,49.1875000013656,-1.28537377788739E-14));
#5771=CARTESIAN_POINT('',(-104.958734125,49.4375000013656,0.));
#5772=CARTESIAN_POINT('',(-104.958734125,49.4375000013656,0.));
#5773=CARTESIAN_POINT('Ctrl Pts',(-104.958734125,49.4375000013656,0.));
#5774=CARTESIAN_POINT('Ctrl Pts',(-104.958734125,49.3750000013656,-43.4753311640868));
#5775=CARTESIAN_POINT('Ctrl Pts',(-74.2170326445434,49.3125000013656,-74.2170326445434));
#5776=CARTESIAN_POINT('Ctrl Pts',(-43.4753311640868,49.2500000013656,-104.958734125));
#5777=CARTESIAN_POINT('Ctrl Pts',(-6.42686888943697E-15,49.1875000013656,
-104.958734125));
#5778=CARTESIAN_POINT('Ctrl Pts',(43.4753311640868,49.1250000013656,-104.958734125));
#5779=CARTESIAN_POINT('Ctrl Pts',(74.2170326445434,49.0625000013656,-74.2170326445434));
#5780=CARTESIAN_POINT('Ctrl Pts',(104.958734125,49.0000000013656,-43.4753311640868));
#5781=CARTESIAN_POINT('Ctrl Pts',(104.958734125,48.9375000013656,-1.28537377788739E-14));
#5782=CARTESIAN_POINT('Origin',(0.,105.,0.));
#5783=CARTESIAN_POINT('',(3.23000593275114E-15,0.375000002731177,105.5));
#5784=CARTESIAN_POINT('',(3.23000593275114E-15,0.249999999999986,105.5));
#5785=CARTESIAN_POINT('',(-1.29200237310046E-14,105.,105.5));
#5786=CARTESIAN_POINT('',(-105.5,0.,0.));
#5787=CARTESIAN_POINT('Ctrl Pts',(1.93800355965069E-14,0.249999999999986,
105.5));
#5788=CARTESIAN_POINT('Ctrl Pts',(-43.6995308303616,0.187499999999986,105.5));
#5789=CARTESIAN_POINT('Ctrl Pts',(-74.5997654151808,0.124999999999986,74.5997654151808));
#5790=CARTESIAN_POINT('Ctrl Pts',(-105.5,0.0624999999999862,43.6995308303616));
#5791=CARTESIAN_POINT('Ctrl Pts',(-105.5,-1.38777878078145E-14,0.));
#5792=CARTESIAN_POINT('',(-74.5997640648779,1.90551595483966E-15,-74.5997667654837));
#5793=CARTESIAN_POINT('Origin',(0.,0.,0.));
#5794=CARTESIAN_POINT('Ctrl Pts',(1.93800355965069E-14,0.375000002731177,
105.5));
#5795=CARTESIAN_POINT('Ctrl Pts',(-43.6995308303616,0.312500002731177,105.5));
#5796=CARTESIAN_POINT('Ctrl Pts',(-74.5997654151808,0.250000002731177,74.5997654151808));
#5797=CARTESIAN_POINT('Ctrl Pts',(-105.5,0.187500002731177,43.6995308303616));
#5798=CARTESIAN_POINT('Ctrl Pts',(-105.5,0.125000002731177,0.));
#5799=CARTESIAN_POINT('Ctrl Pts',(-105.5,0.0625000027311765,-43.6995308303615));
#5800=CARTESIAN_POINT('Ctrl Pts',(-74.5997640648778,1.90551595467487E-15,
-74.5997667654837));
#5801=CARTESIAN_POINT('Origin',(0.,105.,0.));
#5802=CARTESIAN_POINT('',(3.23000593275114E-15,1.37500000273118,105.5));
#5803=CARTESIAN_POINT('',(3.23000593275114E-15,1.24999999999999,105.5));
#5804=CARTESIAN_POINT('',(-1.29200237310046E-14,105.,105.5));
#5805=CARTESIAN_POINT('Ctrl Pts',(1.93800355965069E-14,1.24999999999999,
105.5));
#5806=CARTESIAN_POINT('Ctrl Pts',(-43.6995308303616,1.18749999999999,105.5));
#5807=CARTESIAN_POINT('Ctrl Pts',(-74.5997654151808,1.12499999999999,74.5997654151808));
#5808=CARTESIAN_POINT('Ctrl Pts',(-105.5,1.06249999999999,43.6995308303616));
#5809=CARTESIAN_POINT('Ctrl Pts',(-105.5,0.999999999999987,0.));
#5810=CARTESIAN_POINT('Ctrl Pts',(-105.5,0.937499999999987,-43.6995308303615));
#5811=CARTESIAN_POINT('Ctrl Pts',(-74.5997654151808,0.874999999999987,-74.5997654151808));
#5812=CARTESIAN_POINT('Ctrl Pts',(-43.6995308303615,0.812499999999987,-105.5));
#5813=CARTESIAN_POINT('Ctrl Pts',(-6.46001186550229E-15,0.749999999999987,
-105.5));
#5814=CARTESIAN_POINT('Ctrl Pts',(43.6995308303615,0.687499999999987,-105.5));
#5815=CARTESIAN_POINT('Ctrl Pts',(74.5997654151808,0.624999999999987,-74.5997654151808));
#5816=CARTESIAN_POINT('Ctrl Pts',(105.5,0.562499999999987,-43.6995308303616));
#5817=CARTESIAN_POINT('Ctrl Pts',(105.5,0.499999999999987,-1.29200237310046E-14));
#5818=CARTESIAN_POINT('Ctrl Pts',(105.5,0.437499999999987,43.6995308303615));
#5819=CARTESIAN_POINT('Ctrl Pts',(74.5997654151808,0.374999999999986,74.5997654151808));
#5820=CARTESIAN_POINT('Ctrl Pts',(43.6995308303616,0.312499999999986,105.5));
#5821=CARTESIAN_POINT('Ctrl Pts',(1.93800355965069E-14,0.249999999999986,
105.5));
#5822=CARTESIAN_POINT('Ctrl Pts',(1.93800355965069E-14,1.37500000273118,
105.5));
#5823=CARTESIAN_POINT('Ctrl Pts',(-43.6995308303616,1.31250000273118,105.5));
#5824=CARTESIAN_POINT('Ctrl Pts',(-74.5997654151808,1.25000000273118,74.5997654151808));
#5825=CARTESIAN_POINT('Ctrl Pts',(-105.5,1.18750000273118,43.6995308303616));
#5826=CARTESIAN_POINT('Ctrl Pts',(-105.5,1.12500000273118,0.));
#5827=CARTESIAN_POINT('Ctrl Pts',(-105.5,1.06250000273118,-43.6995308303615));
#5828=CARTESIAN_POINT('Ctrl Pts',(-74.5997654151808,1.00000000273118,-74.5997654151808));
#5829=CARTESIAN_POINT('Ctrl Pts',(-43.6995308303615,0.937500002731177,-105.5));
#5830=CARTESIAN_POINT('Ctrl Pts',(-6.46001186550229E-15,0.875000002731177,
-105.5));
#5831=CARTESIAN_POINT('Ctrl Pts',(43.6995308303615,0.812500002731177,-105.5));
#5832=CARTESIAN_POINT('Ctrl Pts',(74.5997654151808,0.750000002731177,-74.5997654151808));
#5833=CARTESIAN_POINT('Ctrl Pts',(105.5,0.687500002731177,-43.6995308303616));
#5834=CARTESIAN_POINT('Ctrl Pts',(105.5,0.625000002731177,-1.29200237310046E-14));
#5835=CARTESIAN_POINT('Ctrl Pts',(105.5,0.562500002731177,43.6995308303615));
#5836=CARTESIAN_POINT('Ctrl Pts',(74.5997654151808,0.500000002731177,74.5997654151808));
#5837=CARTESIAN_POINT('Ctrl Pts',(43.6995308303616,0.437500002731177,105.5));
#5838=CARTESIAN_POINT('Ctrl Pts',(1.93800355965069E-14,0.375000002731177,
105.5));
#5839=CARTESIAN_POINT('Origin',(0.,105.,0.));
#5840=CARTESIAN_POINT('',(3.23000593275114E-15,2.37500000273118,105.5));
#5841=CARTESIAN_POINT('',(3.23000593275114E-15,2.24999999999999,105.5));
#5842=CARTESIAN_POINT('',(-1.29200237310046E-14,105.,105.5));
#5843=CARTESIAN_POINT('Ctrl Pts',(1.93800355965069E-14,2.24999999999999,
105.5));
#5844=CARTESIAN_POINT('Ctrl Pts',(-43.6995308303616,2.18749999999999,105.5));
#5845=CARTESIAN_POINT('Ctrl Pts',(-74.5997654151808,2.12499999999999,74.5997654151808));
#5846=CARTESIAN_POINT('Ctrl Pts',(-105.5,2.06249999999999,43.6995308303616));
#5847=CARTESIAN_POINT('Ctrl Pts',(-105.5,1.99999999999999,0.));
#5848=CARTESIAN_POINT('Ctrl Pts',(-105.5,1.93749999999999,-43.6995308303615));
#5849=CARTESIAN_POINT('Ctrl Pts',(-74.5997654151808,1.87499999999999,-74.5997654151808));
#5850=CARTESIAN_POINT('Ctrl Pts',(-43.6995308303615,1.81249999999999,-105.5));
#5851=CARTESIAN_POINT('Ctrl Pts',(-6.46001186550229E-15,1.74999999999999,
-105.5));
#5852=CARTESIAN_POINT('Ctrl Pts',(43.6995308303615,1.68749999999999,-105.5));
#5853=CARTESIAN_POINT('Ctrl Pts',(74.5997654151808,1.62499999999999,-74.5997654151808));
#5854=CARTESIAN_POINT('Ctrl Pts',(105.5,1.56249999999999,-43.6995308303616));
#5855=CARTESIAN_POINT('Ctrl Pts',(105.5,1.49999999999999,-1.29200237310046E-14));
#5856=CARTESIAN_POINT('Ctrl Pts',(105.5,1.43749999999999,43.6995308303615));
#5857=CARTESIAN_POINT('Ctrl Pts',(74.5997654151808,1.37499999999999,74.5997654151808));
#5858=CARTESIAN_POINT('Ctrl Pts',(43.6995308303616,1.31249999999999,105.5));
#5859=CARTESIAN_POINT('Ctrl Pts',(1.93800355965069E-14,1.24999999999999,
105.5));
#5860=CARTESIAN_POINT('Ctrl Pts',(1.93800355965069E-14,2.37500000273118,
105.5));
#5861=CARTESIAN_POINT('Ctrl Pts',(-43.6995308303616,2.31250000273118,105.5));
#5862=CARTESIAN_POINT('Ctrl Pts',(-74.5997654151808,2.25000000273118,74.5997654151808));
#5863=CARTESIAN_POINT('Ctrl Pts',(-105.5,2.18750000273118,43.6995308303616));
#5864=CARTESIAN_POINT('Ctrl Pts',(-105.5,2.12500000273118,0.));
#5865=CARTESIAN_POINT('Ctrl Pts',(-105.5,2.06250000273118,-43.6995308303615));
#5866=CARTESIAN_POINT('Ctrl Pts',(-74.5997654151808,2.00000000273118,-74.5997654151808));
#5867=CARTESIAN_POINT('Ctrl Pts',(-43.6995308303615,1.93750000273118,-105.5));
#5868=CARTESIAN_POINT('Ctrl Pts',(-6.46001186550229E-15,1.87500000273118,
-105.5));
#5869=CARTESIAN_POINT('Ctrl Pts',(43.6995308303615,1.81250000273118,-105.5));
#5870=CARTESIAN_POINT('Ctrl Pts',(74.5997654151808,1.75000000273118,-74.5997654151808));
#5871=CARTESIAN_POINT('Ctrl Pts',(105.5,1.68750000273118,-43.6995308303616));
#5872=CARTESIAN_POINT('Ctrl Pts',(105.5,1.62500000273118,-1.29200237310046E-14));
#5873=CARTESIAN_POINT('Ctrl Pts',(105.5,1.56250000273118,43.6995308303615));
#5874=CARTESIAN_POINT('Ctrl Pts',(74.5997654151808,1.50000000273118,74.5997654151808));
#5875=CARTESIAN_POINT('Ctrl Pts',(43.6995308303616,1.43750000273118,105.5));
#5876=CARTESIAN_POINT('Ctrl Pts',(1.93800355965069E-14,1.37500000273118,
105.5));
#5877=CARTESIAN_POINT('Origin',(0.,105.,0.));
#5878=CARTESIAN_POINT('',(3.23000593275114E-15,3.37500000273118,105.5));
#5879=CARTESIAN_POINT('',(3.23000593275114E-15,3.24999999999999,105.5));
#5880=CARTESIAN_POINT('',(-1.29200237310046E-14,105.,105.5));
#5881=CARTESIAN_POINT('Ctrl Pts',(1.93800355965069E-14,3.24999999999999,
105.5));
#5882=CARTESIAN_POINT('Ctrl Pts',(-43.6995308303616,3.18749999999999,105.5));
#5883=CARTESIAN_POINT('Ctrl Pts',(-74.5997654151808,3.12499999999999,74.5997654151808));
#5884=CARTESIAN_POINT('Ctrl Pts',(-105.5,3.06249999999999,43.6995308303616));
#5885=CARTESIAN_POINT('Ctrl Pts',(-105.5,2.99999999999999,0.));
#5886=CARTESIAN_POINT('Ctrl Pts',(-105.5,2.93749999999999,-43.6995308303615));
#5887=CARTESIAN_POINT('Ctrl Pts',(-74.5997654151808,2.87499999999999,-74.5997654151808));
#5888=CARTESIAN_POINT('Ctrl Pts',(-43.6995308303615,2.81249999999999,-105.5));
#5889=CARTESIAN_POINT('Ctrl Pts',(-6.46001186550229E-15,2.74999999999999,
-105.5));
#5890=CARTESIAN_POINT('Ctrl Pts',(43.6995308303615,2.68749999999999,-105.5));
#5891=CARTESIAN_POINT('Ctrl Pts',(74.5997654151808,2.62499999999999,-74.5997654151808));
#5892=CARTESIAN_POINT('Ctrl Pts',(105.5,2.56249999999999,-43.6995308303616));
#5893=CARTESIAN_POINT('Ctrl Pts',(105.5,2.49999999999999,-1.29200237310046E-14));
#5894=CARTESIAN_POINT('Ctrl Pts',(105.5,2.43749999999999,43.6995308303615));
#5895=CARTESIAN_POINT('Ctrl Pts',(74.5997654151808,2.37499999999999,74.5997654151808));
#5896=CARTESIAN_POINT('Ctrl Pts',(43.6995308303616,2.31249999999999,105.5));
#5897=CARTESIAN_POINT('Ctrl Pts',(1.93800355965069E-14,2.24999999999999,
105.5));
#5898=CARTESIAN_POINT('Ctrl Pts',(1.93800355965069E-14,3.37500000273118,
105.5));
#5899=CARTESIAN_POINT('Ctrl Pts',(-43.6995308303616,3.31250000273118,105.5));
#5900=CARTESIAN_POINT('Ctrl Pts',(-74.5997654151808,3.25000000273118,74.5997654151808));
#5901=CARTESIAN_POINT('Ctrl Pts',(-105.5,3.18750000273118,43.6995308303616));
#5902=CARTESIAN_POINT('Ctrl Pts',(-105.5,3.12500000273118,0.));
#5903=CARTESIAN_POINT('Ctrl Pts',(-105.5,3.06250000273118,-43.6995308303615));
#5904=CARTESIAN_POINT('Ctrl Pts',(-74.5997654151808,3.00000000273118,-74.5997654151808));
#5905=CARTESIAN_POINT('Ctrl Pts',(-43.6995308303615,2.93750000273118,-105.5));
#5906=CARTESIAN_POINT('Ctrl Pts',(-6.46001186550229E-15,2.87500000273118,
-105.5));
#5907=CARTESIAN_POINT('Ctrl Pts',(43.6995308303615,2.81250000273118,-105.5));
#5908=CARTESIAN_POINT('Ctrl Pts',(74.5997654151808,2.75000000273118,-74.5997654151808));
#5909=CARTESIAN_POINT('Ctrl Pts',(105.5,2.68750000273118,-43.6995308303616));
#5910=CARTESIAN_POINT('Ctrl Pts',(105.5,2.62500000273118,-1.29200237310046E-14));
#5911=CARTESIAN_POINT('Ctrl Pts',(105.5,2.56250000273118,43.6995308303615));
#5912=CARTESIAN_POINT('Ctrl Pts',(74.5997654151808,2.50000000273118,74.5997654151808));
#5913=CARTESIAN_POINT('Ctrl Pts',(43.6995308303616,2.43750000273118,105.5));
#5914=CARTESIAN_POINT('Ctrl Pts',(1.93800355965069E-14,2.37500000273118,
105.5));
#5915=CARTESIAN_POINT('Origin',(0.,105.,0.));
#5916=CARTESIAN_POINT('',(3.23000593275114E-15,4.37500000273118,105.5));
#5917=CARTESIAN_POINT('',(3.23000593275114E-15,4.24999999999999,105.5));
#5918=CARTESIAN_POINT('',(-1.29200237310046E-14,105.,105.5));
#5919=CARTESIAN_POINT('Ctrl Pts',(1.93800355965069E-14,4.24999999999999,
105.5));
#5920=CARTESIAN_POINT('Ctrl Pts',(-43.6995308303616,4.18749999999999,105.5));
#5921=CARTESIAN_POINT('Ctrl Pts',(-74.5997654151808,4.12499999999999,74.5997654151808));
#5922=CARTESIAN_POINT('Ctrl Pts',(-105.5,4.06249999999999,43.6995308303616));
#5923=CARTESIAN_POINT('Ctrl Pts',(-105.5,3.99999999999999,0.));
#5924=CARTESIAN_POINT('Ctrl Pts',(-105.5,3.93749999999999,-43.6995308303615));
#5925=CARTESIAN_POINT('Ctrl Pts',(-74.5997654151808,3.87499999999999,-74.5997654151808));
#5926=CARTESIAN_POINT('Ctrl Pts',(-43.6995308303615,3.81249999999999,-105.5));
#5927=CARTESIAN_POINT('Ctrl Pts',(-6.46001186550229E-15,3.74999999999999,
-105.5));
#5928=CARTESIAN_POINT('Ctrl Pts',(43.6995308303615,3.68749999999999,-105.5));
#5929=CARTESIAN_POINT('Ctrl Pts',(74.5997654151808,3.62499999999999,-74.5997654151808));
#5930=CARTESIAN_POINT('Ctrl Pts',(105.5,3.56249999999999,-43.6995308303616));
#5931=CARTESIAN_POINT('Ctrl Pts',(105.5,3.49999999999999,-1.29200237310046E-14));
#5932=CARTESIAN_POINT('Ctrl Pts',(105.5,3.43749999999999,43.6995308303615));
#5933=CARTESIAN_POINT('Ctrl Pts',(74.5997654151808,3.37499999999999,74.5997654151808));
#5934=CARTESIAN_POINT('Ctrl Pts',(43.6995308303616,3.31249999999999,105.5));
#5935=CARTESIAN_POINT('Ctrl Pts',(1.93800355965069E-14,3.24999999999999,
105.5));
#5936=CARTESIAN_POINT('Ctrl Pts',(1.93800355965069E-14,4.37500000273118,
105.5));
#5937=CARTESIAN_POINT('Ctrl Pts',(-43.6995308303616,4.31250000273118,105.5));
#5938=CARTESIAN_POINT('Ctrl Pts',(-74.5997654151808,4.25000000273118,74.5997654151808));
#5939=CARTESIAN_POINT('Ctrl Pts',(-105.5,4.18750000273118,43.6995308303616));
#5940=CARTESIAN_POINT('Ctrl Pts',(-105.5,4.12500000273118,0.));
#5941=CARTESIAN_POINT('Ctrl Pts',(-105.5,4.06250000273118,-43.6995308303615));
#5942=CARTESIAN_POINT('Ctrl Pts',(-74.5997654151808,4.00000000273118,-74.5997654151808));
#5943=CARTESIAN_POINT('Ctrl Pts',(-43.6995308303615,3.93750000273118,-105.5));
#5944=CARTESIAN_POINT('Ctrl Pts',(-6.46001186550229E-15,3.87500000273118,
-105.5));
#5945=CARTESIAN_POINT('Ctrl Pts',(43.6995308303615,3.81250000273118,-105.5));
#5946=CARTESIAN_POINT('Ctrl Pts',(74.5997654151808,3.75000000273118,-74.5997654151808));
#5947=CARTESIAN_POINT('Ctrl Pts',(105.5,3.68750000273118,-43.6995308303616));
#5948=CARTESIAN_POINT('Ctrl Pts',(105.5,3.62500000273118,-1.29200237310046E-14));
#5949=CARTESIAN_POINT('Ctrl Pts',(105.5,3.56250000273118,43.6995308303615));
#5950=CARTESIAN_POINT('Ctrl Pts',(74.5997654151808,3.50000000273118,74.5997654151808));
#5951=CARTESIAN_POINT('Ctrl Pts',(43.6995308303616,3.43750000273118,105.5));
#5952=CARTESIAN_POINT('Ctrl Pts',(1.93800355965069E-14,3.37500000273118,
105.5));
#5953=CARTESIAN_POINT('Origin',(0.,105.,0.));
#5954=CARTESIAN_POINT('',(3.23000593275114E-15,5.37500000273117,105.5));
#5955=CARTESIAN_POINT('',(3.23000593275114E-15,5.24999999999999,105.5));
#5956=CARTESIAN_POINT('',(-1.29200237310046E-14,105.,105.5));
#5957=CARTESIAN_POINT('Ctrl Pts',(1.93800355965069E-14,5.24999999999999,
105.5));
#5958=CARTESIAN_POINT('Ctrl Pts',(-43.6995308303616,5.18749999999999,105.5));
#5959=CARTESIAN_POINT('Ctrl Pts',(-74.5997654151808,5.12499999999999,74.5997654151808));
#5960=CARTESIAN_POINT('Ctrl Pts',(-105.5,5.06249999999999,43.6995308303616));
#5961=CARTESIAN_POINT('Ctrl Pts',(-105.5,4.99999999999999,0.));
#5962=CARTESIAN_POINT('Ctrl Pts',(-105.5,4.93749999999999,-43.6995308303615));
#5963=CARTESIAN_POINT('Ctrl Pts',(-74.5997654151808,4.87499999999999,-74.5997654151808));
#5964=CARTESIAN_POINT('Ctrl Pts',(-43.6995308303615,4.81249999999999,-105.5));
#5965=CARTESIAN_POINT('Ctrl Pts',(-6.46001186550229E-15,4.74999999999999,
-105.5));
#5966=CARTESIAN_POINT('Ctrl Pts',(43.6995308303615,4.68749999999999,-105.5));
#5967=CARTESIAN_POINT('Ctrl Pts',(74.5997654151808,4.62499999999999,-74.5997654151808));
#5968=CARTESIAN_POINT('Ctrl Pts',(105.5,4.56249999999999,-43.6995308303616));
#5969=CARTESIAN_POINT('Ctrl Pts',(105.5,4.49999999999999,-1.29200237310046E-14));
#5970=CARTESIAN_POINT('Ctrl Pts',(105.5,4.43749999999999,43.6995308303615));
#5971=CARTESIAN_POINT('Ctrl Pts',(74.5997654151808,4.37499999999999,74.5997654151808));
#5972=CARTESIAN_POINT('Ctrl Pts',(43.6995308303616,4.31249999999999,105.5));
#5973=CARTESIAN_POINT('Ctrl Pts',(1.93800355965069E-14,4.24999999999999,
105.5));
#5974=CARTESIAN_POINT('Ctrl Pts',(1.93800355965069E-14,5.37500000273117,
105.5));
#5975=CARTESIAN_POINT('Ctrl Pts',(-43.6995308303616,5.31250000273117,105.5));
#5976=CARTESIAN_POINT('Ctrl Pts',(-74.5997654151808,5.25000000273117,74.5997654151808));
#5977=CARTESIAN_POINT('Ctrl Pts',(-105.5,5.18750000273117,43.6995308303616));
#5978=CARTESIAN_POINT('Ctrl Pts',(-105.5,5.12500000273118,0.));
#5979=CARTESIAN_POINT('Ctrl Pts',(-105.5,5.06250000273118,-43.6995308303615));
#5980=CARTESIAN_POINT('Ctrl Pts',(-74.5997654151808,5.00000000273118,-74.5997654151808));
#5981=CARTESIAN_POINT('Ctrl Pts',(-43.6995308303615,4.93750000273118,-105.5));
#5982=CARTESIAN_POINT('Ctrl Pts',(-6.46001186550229E-15,4.87500000273118,
-105.5));
#5983=CARTESIAN_POINT('Ctrl Pts',(43.6995308303615,4.81250000273118,-105.5));
#5984=CARTESIAN_POINT('Ctrl Pts',(74.5997654151808,4.75000000273118,-74.5997654151808));
#5985=CARTESIAN_POINT('Ctrl Pts',(105.5,4.68750000273118,-43.6995308303616));
#5986=CARTESIAN_POINT('Ctrl Pts',(105.5,4.62500000273118,-1.29200237310046E-14));
#5987=CARTESIAN_POINT('Ctrl Pts',(105.5,4.56250000273118,43.6995308303615));
#5988=CARTESIAN_POINT('Ctrl Pts',(74.5997654151808,4.50000000273118,74.5997654151808));
#5989=CARTESIAN_POINT('Ctrl Pts',(43.6995308303616,4.43750000273118,105.5));
#5990=CARTESIAN_POINT('Ctrl Pts',(1.93800355965069E-14,4.37500000273118,
105.5));
#5991=CARTESIAN_POINT('Origin',(0.,105.,0.));
#5992=CARTESIAN_POINT('',(3.23000593275114E-15,6.37500000273118,105.5));
#5993=CARTESIAN_POINT('',(3.23000593275114E-15,6.24999999999998,105.5));
#5994=CARTESIAN_POINT('',(-1.29200237310046E-14,105.,105.5));
#5995=CARTESIAN_POINT('Ctrl Pts',(1.93800355965069E-14,6.24999999999998,
105.5));
#5996=CARTESIAN_POINT('Ctrl Pts',(-43.6995308303616,6.18749999999998,105.5));
#5997=CARTESIAN_POINT('Ctrl Pts',(-74.5997654151808,6.12499999999998,74.5997654151808));
#5998=CARTESIAN_POINT('Ctrl Pts',(-105.5,6.06249999999998,43.6995308303616));
#5999=CARTESIAN_POINT('Ctrl Pts',(-105.5,5.99999999999999,0.));
#6000=CARTESIAN_POINT('Ctrl Pts',(-105.5,5.93749999999999,-43.6995308303615));
#6001=CARTESIAN_POINT('Ctrl Pts',(-74.5997654151808,5.87499999999999,-74.5997654151808));
#6002=CARTESIAN_POINT('Ctrl Pts',(-43.6995308303615,5.81249999999999,-105.5));
#6003=CARTESIAN_POINT('Ctrl Pts',(-6.46001186550229E-15,5.74999999999999,
-105.5));
#6004=CARTESIAN_POINT('Ctrl Pts',(43.6995308303615,5.68749999999999,-105.5));
#6005=CARTESIAN_POINT('Ctrl Pts',(74.5997654151808,5.62499999999999,-74.5997654151808));
#6006=CARTESIAN_POINT('Ctrl Pts',(105.5,5.56249999999999,-43.6995308303616));
#6007=CARTESIAN_POINT('Ctrl Pts',(105.5,5.49999999999999,-1.29200237310046E-14));
#6008=CARTESIAN_POINT('Ctrl Pts',(105.5,5.43749999999999,43.6995308303615));
#6009=CARTESIAN_POINT('Ctrl Pts',(74.5997654151808,5.37499999999999,74.5997654151808));
#6010=CARTESIAN_POINT('Ctrl Pts',(43.6995308303616,5.31249999999999,105.5));
#6011=CARTESIAN_POINT('Ctrl Pts',(1.93800355965069E-14,5.24999999999999,
105.5));
#6012=CARTESIAN_POINT('Ctrl Pts',(1.93800355965069E-14,6.37500000273118,
105.5));
#6013=CARTESIAN_POINT('Ctrl Pts',(-43.6995308303616,6.31250000273118,105.5));
#6014=CARTESIAN_POINT('Ctrl Pts',(-74.5997654151808,6.25000000273118,74.5997654151808));
#6015=CARTESIAN_POINT('Ctrl Pts',(-105.5,6.18750000273117,43.6995308303616));
#6016=CARTESIAN_POINT('Ctrl Pts',(-105.5,6.12500000273117,0.));
#6017=CARTESIAN_POINT('Ctrl Pts',(-105.5,6.06250000273118,-43.6995308303615));
#6018=CARTESIAN_POINT('Ctrl Pts',(-74.5997654151808,6.00000000273118,-74.5997654151808));
#6019=CARTESIAN_POINT('Ctrl Pts',(-43.6995308303615,5.93750000273118,-105.5));
#6020=CARTESIAN_POINT('Ctrl Pts',(-6.46001186550229E-15,5.87500000273117,
-105.5));
#6021=CARTESIAN_POINT('Ctrl Pts',(43.6995308303615,5.81250000273117,-105.5));
#6022=CARTESIAN_POINT('Ctrl Pts',(74.5997654151808,5.75000000273118,-74.5997654151808));
#6023=CARTESIAN_POINT('Ctrl Pts',(105.5,5.68750000273117,-43.6995308303616));
#6024=CARTESIAN_POINT('Ctrl Pts',(105.5,5.62500000273117,-1.29200237310046E-14));
#6025=CARTESIAN_POINT('Ctrl Pts',(105.5,5.56250000273117,43.6995308303615));
#6026=CARTESIAN_POINT('Ctrl Pts',(74.5997654151808,5.50000000273117,74.5997654151808));
#6027=CARTESIAN_POINT('Ctrl Pts',(43.6995308303616,5.43750000273118,105.5));
#6028=CARTESIAN_POINT('Ctrl Pts',(1.93800355965069E-14,5.37500000273117,
105.5));
#6029=CARTESIAN_POINT('Origin',(0.,105.,0.));
#6030=CARTESIAN_POINT('',(3.23000593275114E-15,7.37500000273118,105.5));
#6031=CARTESIAN_POINT('',(3.23000593275114E-15,7.24999999999999,105.5));
#6032=CARTESIAN_POINT('',(-1.29200237310046E-14,105.,105.5));
#6033=CARTESIAN_POINT('Ctrl Pts',(1.93800355965069E-14,7.24999999999999,
105.5));
#6034=CARTESIAN_POINT('Ctrl Pts',(-43.6995308303616,7.18749999999999,105.5));
#6035=CARTESIAN_POINT('Ctrl Pts',(-74.5997654151808,7.12499999999999,74.5997654151808));
#6036=CARTESIAN_POINT('Ctrl Pts',(-105.5,7.06249999999998,43.6995308303616));
#6037=CARTESIAN_POINT('Ctrl Pts',(-105.5,6.99999999999998,0.));
#6038=CARTESIAN_POINT('Ctrl Pts',(-105.5,6.93749999999999,-43.6995308303615));
#6039=CARTESIAN_POINT('Ctrl Pts',(-74.5997654151808,6.87499999999999,-74.5997654151808));
#6040=CARTESIAN_POINT('Ctrl Pts',(-43.6995308303615,6.81249999999999,-105.5));
#6041=CARTESIAN_POINT('Ctrl Pts',(-6.46001186550229E-15,6.74999999999998,
-105.5));
#6042=CARTESIAN_POINT('Ctrl Pts',(43.6995308303615,6.68749999999998,-105.5));
#6043=CARTESIAN_POINT('Ctrl Pts',(74.5997654151808,6.62499999999999,-74.5997654151808));
#6044=CARTESIAN_POINT('Ctrl Pts',(105.5,6.56249999999998,-43.6995308303616));
#6045=CARTESIAN_POINT('Ctrl Pts',(105.5,6.49999999999998,-1.29200237310046E-14));
#6046=CARTESIAN_POINT('Ctrl Pts',(105.5,6.43749999999998,43.6995308303615));
#6047=CARTESIAN_POINT('Ctrl Pts',(74.5997654151808,6.37499999999998,74.5997654151808));
#6048=CARTESIAN_POINT('Ctrl Pts',(43.6995308303616,6.31249999999999,105.5));
#6049=CARTESIAN_POINT('Ctrl Pts',(1.93800355965069E-14,6.24999999999998,
105.5));
#6050=CARTESIAN_POINT('Ctrl Pts',(1.93800355965069E-14,7.37500000273118,
105.5));
#6051=CARTESIAN_POINT('Ctrl Pts',(-43.6995308303616,7.31250000273118,105.5));
#6052=CARTESIAN_POINT('Ctrl Pts',(-74.5997654151808,7.25000000273118,74.5997654151808));
#6053=CARTESIAN_POINT('Ctrl Pts',(-105.5,7.18750000273118,43.6995308303616));
#6054=CARTESIAN_POINT('Ctrl Pts',(-105.5,7.12500000273118,0.));
#6055=CARTESIAN_POINT('Ctrl Pts',(-105.5,7.06250000273118,-43.6995308303615));
#6056=CARTESIAN_POINT('Ctrl Pts',(-74.5997654151808,7.00000000273118,-74.5997654151808));
#6057=CARTESIAN_POINT('Ctrl Pts',(-43.6995308303615,6.93750000273118,-105.5));
#6058=CARTESIAN_POINT('Ctrl Pts',(-6.46001186550229E-15,6.87500000273118,
-105.5));
#6059=CARTESIAN_POINT('Ctrl Pts',(43.6995308303615,6.81250000273118,-105.5));
#6060=CARTESIAN_POINT('Ctrl Pts',(74.5997654151808,6.75000000273118,-74.5997654151808));
#6061=CARTESIAN_POINT('Ctrl Pts',(105.5,6.68750000273118,-43.6995308303616));
#6062=CARTESIAN_POINT('Ctrl Pts',(105.5,6.62500000273118,-1.29200237310046E-14));
#6063=CARTESIAN_POINT('Ctrl Pts',(105.5,6.56250000273118,43.6995308303615));
#6064=CARTESIAN_POINT('Ctrl Pts',(74.5997654151808,6.50000000273118,74.5997654151808));
#6065=CARTESIAN_POINT('Ctrl Pts',(43.6995308303616,6.43750000273118,105.5));
#6066=CARTESIAN_POINT('Ctrl Pts',(1.93800355965069E-14,6.37500000273118,
105.5));
#6067=CARTESIAN_POINT('Origin',(0.,105.,0.));
#6068=CARTESIAN_POINT('',(3.23000593275114E-15,8.37500000273118,105.5));
#6069=CARTESIAN_POINT('',(3.23000593275114E-15,8.24999999999999,105.5));
#6070=CARTESIAN_POINT('',(-1.29200237310046E-14,105.,105.5));
#6071=CARTESIAN_POINT('Ctrl Pts',(1.93800355965069E-14,8.24999999999999,
105.5));
#6072=CARTESIAN_POINT('Ctrl Pts',(-43.6995308303616,8.18749999999999,105.5));
#6073=CARTESIAN_POINT('Ctrl Pts',(-74.5997654151808,8.12499999999999,74.5997654151808));
#6074=CARTESIAN_POINT('Ctrl Pts',(-105.5,8.06249999999999,43.6995308303616));
#6075=CARTESIAN_POINT('Ctrl Pts',(-105.5,7.99999999999999,0.));
#6076=CARTESIAN_POINT('Ctrl Pts',(-105.5,7.93749999999999,-43.6995308303615));
#6077=CARTESIAN_POINT('Ctrl Pts',(-74.5997654151808,7.87499999999999,-74.5997654151808));
#6078=CARTESIAN_POINT('Ctrl Pts',(-43.6995308303615,7.81249999999999,-105.5));
#6079=CARTESIAN_POINT('Ctrl Pts',(-6.46001186550229E-15,7.74999999999999,
-105.5));
#6080=CARTESIAN_POINT('Ctrl Pts',(43.6995308303615,7.68749999999999,-105.5));
#6081=CARTESIAN_POINT('Ctrl Pts',(74.5997654151808,7.62499999999999,-74.5997654151808));
#6082=CARTESIAN_POINT('Ctrl Pts',(105.5,7.56249999999999,-43.6995308303616));
#6083=CARTESIAN_POINT('Ctrl Pts',(105.5,7.49999999999999,-1.29200237310046E-14));
#6084=CARTESIAN_POINT('Ctrl Pts',(105.5,7.43749999999999,43.6995308303615));
#6085=CARTESIAN_POINT('Ctrl Pts',(74.5997654151808,7.37499999999999,74.5997654151808));
#6086=CARTESIAN_POINT('Ctrl Pts',(43.6995308303616,7.31249999999999,105.5));
#6087=CARTESIAN_POINT('Ctrl Pts',(1.93800355965069E-14,7.24999999999999,
105.5));
#6088=CARTESIAN_POINT('Ctrl Pts',(1.93800355965069E-14,8.37500000273118,
105.5));
#6089=CARTESIAN_POINT('Ctrl Pts',(-43.6995308303616,8.31250000273118,105.5));
#6090=CARTESIAN_POINT('Ctrl Pts',(-74.5997654151808,8.25000000273118,74.5997654151808));
#6091=CARTESIAN_POINT('Ctrl Pts',(-105.5,8.18750000273118,43.6995308303616));
#6092=CARTESIAN_POINT('Ctrl Pts',(-105.5,8.12500000273118,0.));
#6093=CARTESIAN_POINT('Ctrl Pts',(-105.5,8.06250000273118,-43.6995308303615));
#6094=CARTESIAN_POINT('Ctrl Pts',(-74.5997654151808,8.00000000273118,-74.5997654151808));
#6095=CARTESIAN_POINT('Ctrl Pts',(-43.6995308303615,7.93750000273118,-105.5));
#6096=CARTESIAN_POINT('Ctrl Pts',(-6.46001186550229E-15,7.87500000273118,
-105.5));
#6097=CARTESIAN_POINT('Ctrl Pts',(43.6995308303615,7.81250000273118,-105.5));
#6098=CARTESIAN_POINT('Ctrl Pts',(74.5997654151808,7.75000000273118,-74.5997654151808));
#6099=CARTESIAN_POINT('Ctrl Pts',(105.5,7.68750000273118,-43.6995308303616));
#6100=CARTESIAN_POINT('Ctrl Pts',(105.5,7.62500000273118,-1.29200237310046E-14));
#6101=CARTESIAN_POINT('Ctrl Pts',(105.5,7.56250000273118,43.6995308303615));
#6102=CARTESIAN_POINT('Ctrl Pts',(74.5997654151808,7.50000000273118,74.5997654151808));
#6103=CARTESIAN_POINT('Ctrl Pts',(43.6995308303616,7.43750000273118,105.5));
#6104=CARTESIAN_POINT('Ctrl Pts',(1.93800355965069E-14,7.37500000273118,
105.5));
#6105=CARTESIAN_POINT('Origin',(0.,105.,0.));
#6106=CARTESIAN_POINT('',(3.23000593275114E-15,9.37500000273118,105.5));
#6107=CARTESIAN_POINT('',(3.23000593275114E-15,9.24999999999999,105.5));
#6108=CARTESIAN_POINT('',(-1.29200237310046E-14,105.,105.5));
#6109=CARTESIAN_POINT('Ctrl Pts',(1.93800355965069E-14,9.24999999999999,
105.5));
#6110=CARTESIAN_POINT('Ctrl Pts',(-43.6995308303616,9.18749999999999,105.5));
#6111=CARTESIAN_POINT('Ctrl Pts',(-74.5997654151808,9.12499999999999,74.5997654151808));
#6112=CARTESIAN_POINT('Ctrl Pts',(-105.5,9.06249999999999,43.6995308303616));
#6113=CARTESIAN_POINT('Ctrl Pts',(-105.5,8.99999999999999,0.));
#6114=CARTESIAN_POINT('Ctrl Pts',(-105.5,8.93749999999999,-43.6995308303615));
#6115=CARTESIAN_POINT('Ctrl Pts',(-74.5997654151808,8.87499999999999,-74.5997654151808));
#6116=CARTESIAN_POINT('Ctrl Pts',(-43.6995308303615,8.81249999999999,-105.5));
#6117=CARTESIAN_POINT('Ctrl Pts',(-6.46001186550229E-15,8.74999999999999,
-105.5));
#6118=CARTESIAN_POINT('Ctrl Pts',(43.6995308303615,8.68749999999999,-105.5));
#6119=CARTESIAN_POINT('Ctrl Pts',(74.5997654151808,8.62499999999999,-74.5997654151808));
#6120=CARTESIAN_POINT('Ctrl Pts',(105.5,8.56249999999999,-43.6995308303616));
#6121=CARTESIAN_POINT('Ctrl Pts',(105.5,8.49999999999999,-1.29200237310046E-14));
#6122=CARTESIAN_POINT('Ctrl Pts',(105.5,8.43749999999999,43.6995308303615));
#6123=CARTESIAN_POINT('Ctrl Pts',(74.5997654151808,8.37499999999999,74.5997654151808));
#6124=CARTESIAN_POINT('Ctrl Pts',(43.6995308303616,8.31249999999999,105.5));
#6125=CARTESIAN_POINT('Ctrl Pts',(1.93800355965069E-14,8.24999999999999,
105.5));
#6126=CARTESIAN_POINT('Ctrl Pts',(1.93800355965069E-14,9.37500000273118,
105.5));
#6127=CARTESIAN_POINT('Ctrl Pts',(-43.6995308303616,9.31250000273118,105.5));
#6128=CARTESIAN_POINT('Ctrl Pts',(-74.5997654151808,9.25000000273118,74.5997654151808));
#6129=CARTESIAN_POINT('Ctrl Pts',(-105.5,9.18750000273118,43.6995308303616));
#6130=CARTESIAN_POINT('Ctrl Pts',(-105.5,9.12500000273118,0.));
#6131=CARTESIAN_POINT('Ctrl Pts',(-105.5,9.06250000273118,-43.6995308303615));
#6132=CARTESIAN_POINT('Ctrl Pts',(-74.5997654151808,9.00000000273118,-74.5997654151808));
#6133=CARTESIAN_POINT('Ctrl Pts',(-43.6995308303615,8.93750000273118,-105.5));
#6134=CARTESIAN_POINT('Ctrl Pts',(-6.46001186550229E-15,8.87500000273118,
-105.5));
#6135=CARTESIAN_POINT('Ctrl Pts',(43.6995308303615,8.81250000273118,-105.5));
#6136=CARTESIAN_POINT('Ctrl Pts',(74.5997654151808,8.75000000273118,-74.5997654151808));
#6137=CARTESIAN_POINT('Ctrl Pts',(105.5,8.68750000273118,-43.6995308303616));
#6138=CARTESIAN_POINT('Ctrl Pts',(105.5,8.62500000273118,-1.29200237310046E-14));
#6139=CARTESIAN_POINT('Ctrl Pts',(105.5,8.56250000273118,43.6995308303615));
#6140=CARTESIAN_POINT('Ctrl Pts',(74.5997654151808,8.50000000273118,74.5997654151808));
#6141=CARTESIAN_POINT('Ctrl Pts',(43.6995308303616,8.43750000273118,105.5));
#6142=CARTESIAN_POINT('Ctrl Pts',(1.93800355965069E-14,8.37500000273118,
105.5));
#6143=CARTESIAN_POINT('Origin',(0.,105.,0.));
#6144=CARTESIAN_POINT('',(3.23000593275114E-15,10.3750000027312,105.5));
#6145=CARTESIAN_POINT('',(3.23000593275114E-15,10.25,105.5));
#6146=CARTESIAN_POINT('',(-1.29200237310046E-14,105.,105.5));
#6147=CARTESIAN_POINT('Ctrl Pts',(1.93800355965069E-14,10.25,105.5));
#6148=CARTESIAN_POINT('Ctrl Pts',(-43.6995308303616,10.1875,105.5));
#6149=CARTESIAN_POINT('Ctrl Pts',(-74.5997654151808,10.125,74.5997654151808));
#6150=CARTESIAN_POINT('Ctrl Pts',(-105.5,10.0625,43.6995308303616));
#6151=CARTESIAN_POINT('Ctrl Pts',(-105.5,9.99999999999999,0.));
#6152=CARTESIAN_POINT('Ctrl Pts',(-105.5,9.93749999999999,-43.6995308303615));
#6153=CARTESIAN_POINT('Ctrl Pts',(-74.5997654151808,9.87499999999999,-74.5997654151808));
#6154=CARTESIAN_POINT('Ctrl Pts',(-43.6995308303615,9.81249999999999,-105.5));
#6155=CARTESIAN_POINT('Ctrl Pts',(-6.46001186550229E-15,9.74999999999999,
-105.5));
#6156=CARTESIAN_POINT('Ctrl Pts',(43.6995308303615,9.68749999999999,-105.5));
#6157=CARTESIAN_POINT('Ctrl Pts',(74.5997654151808,9.62499999999999,-74.5997654151808));
#6158=CARTESIAN_POINT('Ctrl Pts',(105.5,9.56249999999999,-43.6995308303616));
#6159=CARTESIAN_POINT('Ctrl Pts',(105.5,9.49999999999999,-1.29200237310046E-14));
#6160=CARTESIAN_POINT('Ctrl Pts',(105.5,9.43749999999999,43.6995308303615));
#6161=CARTESIAN_POINT('Ctrl Pts',(74.5997654151808,9.37499999999999,74.5997654151808));
#6162=CARTESIAN_POINT('Ctrl Pts',(43.6995308303616,9.31249999999999,105.5));
#6163=CARTESIAN_POINT('Ctrl Pts',(1.93800355965069E-14,9.24999999999999,
105.5));
#6164=CARTESIAN_POINT('Ctrl Pts',(1.93800355965069E-14,10.3750000027312,
105.5));
#6165=CARTESIAN_POINT('Ctrl Pts',(-43.6995308303616,10.3125000027312,105.5));
#6166=CARTESIAN_POINT('Ctrl Pts',(-74.5997654151808,10.2500000027312,74.5997654151808));
#6167=CARTESIAN_POINT('Ctrl Pts',(-105.5,10.1875000027312,43.6995308303616));
#6168=CARTESIAN_POINT('Ctrl Pts',(-105.5,10.1250000027312,0.));
#6169=CARTESIAN_POINT('Ctrl Pts',(-105.5,10.0625000027312,-43.6995308303615));
#6170=CARTESIAN_POINT('Ctrl Pts',(-74.5997654151808,10.0000000027312,-74.5997654151808));
#6171=CARTESIAN_POINT('Ctrl Pts',(-43.6995308303615,9.93750000273118,-105.5));
#6172=CARTESIAN_POINT('Ctrl Pts',(-6.46001186550229E-15,9.87500000273118,
-105.5));
#6173=CARTESIAN_POINT('Ctrl Pts',(43.6995308303615,9.81250000273118,-105.5));
#6174=CARTESIAN_POINT('Ctrl Pts',(74.5997654151808,9.75000000273118,-74.5997654151808));
#6175=CARTESIAN_POINT('Ctrl Pts',(105.5,9.68750000273118,-43.6995308303616));
#6176=CARTESIAN_POINT('Ctrl Pts',(105.5,9.62500000273118,-1.29200237310046E-14));
#6177=CARTESIAN_POINT('Ctrl Pts',(105.5,9.56250000273118,43.6995308303615));
#6178=CARTESIAN_POINT('Ctrl Pts',(74.5997654151808,9.50000000273118,74.5997654151808));
#6179=CARTESIAN_POINT('Ctrl Pts',(43.6995308303616,9.43750000273118,105.5));
#6180=CARTESIAN_POINT('Ctrl Pts',(1.93800355965069E-14,9.37500000273118,
105.5));
#6181=CARTESIAN_POINT('Origin',(0.,105.,0.));
#6182=CARTESIAN_POINT('',(3.23000593275114E-15,11.3750000027312,105.5));
#6183=CARTESIAN_POINT('',(3.23000593275114E-15,11.25,105.5));
#6184=CARTESIAN_POINT('',(-1.29200237310046E-14,105.,105.5));
#6185=CARTESIAN_POINT('Ctrl Pts',(1.93800355965069E-14,11.25,105.5));
#6186=CARTESIAN_POINT('Ctrl Pts',(-43.6995308303616,11.1875,105.5));
#6187=CARTESIAN_POINT('Ctrl Pts',(-74.5997654151808,11.125,74.5997654151808));
#6188=CARTESIAN_POINT('Ctrl Pts',(-105.5,11.0625,43.6995308303616));
#6189=CARTESIAN_POINT('Ctrl Pts',(-105.5,11.,0.));
#6190=CARTESIAN_POINT('Ctrl Pts',(-105.5,10.9375,-43.6995308303615));
#6191=CARTESIAN_POINT('Ctrl Pts',(-74.5997654151808,10.875,-74.5997654151808));
#6192=CARTESIAN_POINT('Ctrl Pts',(-43.6995308303615,10.8125,-105.5));
#6193=CARTESIAN_POINT('Ctrl Pts',(-6.46001186550229E-15,10.75,-105.5));
#6194=CARTESIAN_POINT('Ctrl Pts',(43.6995308303615,10.6875,-105.5));
#6195=CARTESIAN_POINT('Ctrl Pts',(74.5997654151808,10.625,-74.5997654151808));
#6196=CARTESIAN_POINT('Ctrl Pts',(105.5,10.5625,-43.6995308303616));
#6197=CARTESIAN_POINT('Ctrl Pts',(105.5,10.5,-1.29200237310046E-14));
#6198=CARTESIAN_POINT('Ctrl Pts',(105.5,10.4375,43.6995308303615));
#6199=CARTESIAN_POINT('Ctrl Pts',(74.5997654151808,10.375,74.5997654151808));
#6200=CARTESIAN_POINT('Ctrl Pts',(43.6995308303616,10.3125,105.5));
#6201=CARTESIAN_POINT('Ctrl Pts',(1.93800355965069E-14,10.25,105.5));
#6202=CARTESIAN_POINT('Ctrl Pts',(1.93800355965069E-14,11.3750000027312,
105.5));
#6203=CARTESIAN_POINT('Ctrl Pts',(-43.6995308303616,11.3125000027312,105.5));
#6204=CARTESIAN_POINT('Ctrl Pts',(-74.5997654151808,11.2500000027312,74.5997654151808));
#6205=CARTESIAN_POINT('Ctrl Pts',(-105.5,11.1875000027312,43.6995308303616));
#6206=CARTESIAN_POINT('Ctrl Pts',(-105.5,11.1250000027312,0.));
#6207=CARTESIAN_POINT('Ctrl Pts',(-105.5,11.0625000027312,-43.6995308303615));
#6208=CARTESIAN_POINT('Ctrl Pts',(-74.5997654151808,11.0000000027312,-74.5997654151808));
#6209=CARTESIAN_POINT('Ctrl Pts',(-43.6995308303615,10.9375000027312,-105.5));
#6210=CARTESIAN_POINT('Ctrl Pts',(-6.46001186550229E-15,10.8750000027312,
-105.5));
#6211=CARTESIAN_POINT('Ctrl Pts',(43.6995308303615,10.8125000027312,-105.5));
#6212=CARTESIAN_POINT('Ctrl Pts',(74.5997654151808,10.7500000027312,-74.5997654151808));
#6213=CARTESIAN_POINT('Ctrl Pts',(105.5,10.6875000027312,-43.6995308303616));
#6214=CARTESIAN_POINT('Ctrl Pts',(105.5,10.6250000027312,-1.29200237310046E-14));
#6215=CARTESIAN_POINT('Ctrl Pts',(105.5,10.5625000027312,43.6995308303615));
#6216=CARTESIAN_POINT('Ctrl Pts',(74.5997654151808,10.5000000027312,74.5997654151808));
#6217=CARTESIAN_POINT('Ctrl Pts',(43.6995308303616,10.4375000027312,105.5));
#6218=CARTESIAN_POINT('Ctrl Pts',(1.93800355965069E-14,10.3750000027312,
105.5));
#6219=CARTESIAN_POINT('Origin',(0.,105.,0.));
#6220=CARTESIAN_POINT('',(3.23000593275114E-15,12.3750000027312,105.5));
#6221=CARTESIAN_POINT('',(3.23000593275114E-15,12.25,105.5));
#6222=CARTESIAN_POINT('',(-1.29200237310046E-14,105.,105.5));
#6223=CARTESIAN_POINT('Ctrl Pts',(1.93800355965069E-14,12.25,105.5));
#6224=CARTESIAN_POINT('Ctrl Pts',(-43.6995308303616,12.1875,105.5));
#6225=CARTESIAN_POINT('Ctrl Pts',(-74.5997654151808,12.125,74.5997654151808));
#6226=CARTESIAN_POINT('Ctrl Pts',(-105.5,12.0625,43.6995308303616));
#6227=CARTESIAN_POINT('Ctrl Pts',(-105.5,12.,0.));
#6228=CARTESIAN_POINT('Ctrl Pts',(-105.5,11.9375,-43.6995308303615));
#6229=CARTESIAN_POINT('Ctrl Pts',(-74.5997654151808,11.875,-74.5997654151808));
#6230=CARTESIAN_POINT('Ctrl Pts',(-43.6995308303615,11.8125,-105.5));
#6231=CARTESIAN_POINT('Ctrl Pts',(-6.46001186550229E-15,11.75,-105.5));
#6232=CARTESIAN_POINT('Ctrl Pts',(43.6995308303615,11.6875,-105.5));
#6233=CARTESIAN_POINT('Ctrl Pts',(74.5997654151808,11.625,-74.5997654151808));
#6234=CARTESIAN_POINT('Ctrl Pts',(105.5,11.5625,-43.6995308303616));
#6235=CARTESIAN_POINT('Ctrl Pts',(105.5,11.5,-1.29200237310046E-14));
#6236=CARTESIAN_POINT('Ctrl Pts',(105.5,11.4375,43.6995308303615));
#6237=CARTESIAN_POINT('Ctrl Pts',(74.5997654151808,11.375,74.5997654151808));
#6238=CARTESIAN_POINT('Ctrl Pts',(43.6995308303616,11.3125,105.5));
#6239=CARTESIAN_POINT('Ctrl Pts',(1.93800355965069E-14,11.25,105.5));
#6240=CARTESIAN_POINT('Ctrl Pts',(1.93800355965069E-14,12.3750000027312,
105.5));
#6241=CARTESIAN_POINT('Ctrl Pts',(-43.6995308303616,12.3125000027312,105.5));
#6242=CARTESIAN_POINT('Ctrl Pts',(-74.5997654151808,12.2500000027312,74.5997654151808));
#6243=CARTESIAN_POINT('Ctrl Pts',(-105.5,12.1875000027312,43.6995308303616));
#6244=CARTESIAN_POINT('Ctrl Pts',(-105.5,12.1250000027312,0.));
#6245=CARTESIAN_POINT('Ctrl Pts',(-105.5,12.0625000027312,-43.6995308303615));
#6246=CARTESIAN_POINT('Ctrl Pts',(-74.5997654151808,12.0000000027312,-74.5997654151808));
#6247=CARTESIAN_POINT('Ctrl Pts',(-43.6995308303615,11.9375000027312,-105.5));
#6248=CARTESIAN_POINT('Ctrl Pts',(-6.46001186550229E-15,11.8750000027312,
-105.5));
#6249=CARTESIAN_POINT('Ctrl Pts',(43.6995308303615,11.8125000027312,-105.5));
#6250=CARTESIAN_POINT('Ctrl Pts',(74.5997654151808,11.7500000027312,-74.5997654151808));
#6251=CARTESIAN_POINT('Ctrl Pts',(105.5,11.6875000027312,-43.6995308303616));
#6252=CARTESIAN_POINT('Ctrl Pts',(105.5,11.6250000027312,-1.29200237310046E-14));
#6253=CARTESIAN_POINT('Ctrl Pts',(105.5,11.5625000027312,43.6995308303615));
#6254=CARTESIAN_POINT('Ctrl Pts',(74.5997654151808,11.5000000027312,74.5997654151808));
#6255=CARTESIAN_POINT('Ctrl Pts',(43.6995308303616,11.4375000027312,105.5));
#6256=CARTESIAN_POINT('Ctrl Pts',(1.93800355965069E-14,11.3750000027312,
105.5));
#6257=CARTESIAN_POINT('Origin',(0.,105.,0.));
#6258=CARTESIAN_POINT('',(3.23000593275114E-15,13.3750000027312,105.5));
#6259=CARTESIAN_POINT('',(3.23000593275114E-15,13.25,105.5));
#6260=CARTESIAN_POINT('',(-1.29200237310046E-14,105.,105.5));
#6261=CARTESIAN_POINT('Ctrl Pts',(1.93800355965069E-14,13.25,105.5));
#6262=CARTESIAN_POINT('Ctrl Pts',(-43.6995308303616,13.1875,105.5));
#6263=CARTESIAN_POINT('Ctrl Pts',(-74.5997654151808,13.125,74.5997654151808));
#6264=CARTESIAN_POINT('Ctrl Pts',(-105.5,13.0625,43.6995308303616));
#6265=CARTESIAN_POINT('Ctrl Pts',(-105.5,13.,0.));
#6266=CARTESIAN_POINT('Ctrl Pts',(-105.5,12.9375,-43.6995308303615));
#6267=CARTESIAN_POINT('Ctrl Pts',(-74.5997654151808,12.875,-74.5997654151808));
#6268=CARTESIAN_POINT('Ctrl Pts',(-43.6995308303615,12.8125,-105.5));
#6269=CARTESIAN_POINT('Ctrl Pts',(-6.46001186550229E-15,12.75,-105.5));
#6270=CARTESIAN_POINT('Ctrl Pts',(43.6995308303615,12.6875,-105.5));
#6271=CARTESIAN_POINT('Ctrl Pts',(74.5997654151808,12.625,-74.5997654151808));
#6272=CARTESIAN_POINT('Ctrl Pts',(105.5,12.5625,-43.6995308303616));
#6273=CARTESIAN_POINT('Ctrl Pts',(105.5,12.5,-1.29200237310046E-14));
#6274=CARTESIAN_POINT('Ctrl Pts',(105.5,12.4375,43.6995308303615));
#6275=CARTESIAN_POINT('Ctrl Pts',(74.5997654151808,12.375,74.5997654151808));
#6276=CARTESIAN_POINT('Ctrl Pts',(43.6995308303616,12.3125,105.5));
#6277=CARTESIAN_POINT('Ctrl Pts',(1.93800355965069E-14,12.25,105.5));
#6278=CARTESIAN_POINT('Ctrl Pts',(1.93800355965069E-14,13.3750000027312,
105.5));
#6279=CARTESIAN_POINT('Ctrl Pts',(-43.6995308303616,13.3125000027312,105.5));
#6280=CARTESIAN_POINT('Ctrl Pts',(-74.5997654151808,13.2500000027312,74.5997654151808));
#6281=CARTESIAN_POINT('Ctrl Pts',(-105.5,13.1875000027312,43.6995308303616));
#6282=CARTESIAN_POINT('Ctrl Pts',(-105.5,13.1250000027312,0.));
#6283=CARTESIAN_POINT('Ctrl Pts',(-105.5,13.0625000027312,-43.6995308303615));
#6284=CARTESIAN_POINT('Ctrl Pts',(-74.5997654151808,13.0000000027312,-74.5997654151808));
#6285=CARTESIAN_POINT('Ctrl Pts',(-43.6995308303615,12.9375000027312,-105.5));
#6286=CARTESIAN_POINT('Ctrl Pts',(-6.46001186550229E-15,12.8750000027312,
-105.5));
#6287=CARTESIAN_POINT('Ctrl Pts',(43.6995308303615,12.8125000027312,-105.5));
#6288=CARTESIAN_POINT('Ctrl Pts',(74.5997654151808,12.7500000027312,-74.5997654151808));
#6289=CARTESIAN_POINT('Ctrl Pts',(105.5,12.6875000027312,-43.6995308303616));
#6290=CARTESIAN_POINT('Ctrl Pts',(105.5,12.6250000027312,-1.29200237310046E-14));
#6291=CARTESIAN_POINT('Ctrl Pts',(105.5,12.5625000027312,43.6995308303615));
#6292=CARTESIAN_POINT('Ctrl Pts',(74.5997654151808,12.5000000027312,74.5997654151808));
#6293=CARTESIAN_POINT('Ctrl Pts',(43.6995308303616,12.4375000027312,105.5));
#6294=CARTESIAN_POINT('Ctrl Pts',(1.93800355965069E-14,12.3750000027312,
105.5));
#6295=CARTESIAN_POINT('Origin',(0.,105.,0.));
#6296=CARTESIAN_POINT('',(3.23000593275114E-15,14.3750000027312,105.5));
#6297=CARTESIAN_POINT('',(3.23000593275114E-15,14.25,105.5));
#6298=CARTESIAN_POINT('',(-1.29200237310046E-14,105.,105.5));
#6299=CARTESIAN_POINT('Ctrl Pts',(1.93800355965069E-14,14.25,105.5));
#6300=CARTESIAN_POINT('Ctrl Pts',(-43.6995308303616,14.1875,105.5));
#6301=CARTESIAN_POINT('Ctrl Pts',(-74.5997654151808,14.125,74.5997654151808));
#6302=CARTESIAN_POINT('Ctrl Pts',(-105.5,14.0625,43.6995308303616));
#6303=CARTESIAN_POINT('Ctrl Pts',(-105.5,14.,0.));
#6304=CARTESIAN_POINT('Ctrl Pts',(-105.5,13.9375,-43.6995308303615));
#6305=CARTESIAN_POINT('Ctrl Pts',(-74.5997654151808,13.875,-74.5997654151808));
#6306=CARTESIAN_POINT('Ctrl Pts',(-43.6995308303615,13.8125,-105.5));
#6307=CARTESIAN_POINT('Ctrl Pts',(-6.46001186550229E-15,13.75,-105.5));
#6308=CARTESIAN_POINT('Ctrl Pts',(43.6995308303615,13.6875,-105.5));
#6309=CARTESIAN_POINT('Ctrl Pts',(74.5997654151808,13.625,-74.5997654151808));
#6310=CARTESIAN_POINT('Ctrl Pts',(105.5,13.5625,-43.6995308303616));
#6311=CARTESIAN_POINT('Ctrl Pts',(105.5,13.5,-1.29200237310046E-14));
#6312=CARTESIAN_POINT('Ctrl Pts',(105.5,13.4375,43.6995308303615));
#6313=CARTESIAN_POINT('Ctrl Pts',(74.5997654151808,13.375,74.5997654151808));
#6314=CARTESIAN_POINT('Ctrl Pts',(43.6995308303616,13.3125,105.5));
#6315=CARTESIAN_POINT('Ctrl Pts',(1.93800355965069E-14,13.25,105.5));
#6316=CARTESIAN_POINT('Ctrl Pts',(1.93800355965069E-14,14.3750000027312,
105.5));
#6317=CARTESIAN_POINT('Ctrl Pts',(-43.6995308303616,14.3125000027312,105.5));
#6318=CARTESIAN_POINT('Ctrl Pts',(-74.5997654151808,14.2500000027312,74.5997654151808));
#6319=CARTESIAN_POINT('Ctrl Pts',(-105.5,14.1875000027312,43.6995308303616));
#6320=CARTESIAN_POINT('Ctrl Pts',(-105.5,14.1250000027312,0.));
#6321=CARTESIAN_POINT('Ctrl Pts',(-105.5,14.0625000027312,-43.6995308303615));
#6322=CARTESIAN_POINT('Ctrl Pts',(-74.5997654151808,14.0000000027312,-74.5997654151808));
#6323=CARTESIAN_POINT('Ctrl Pts',(-43.6995308303615,13.9375000027312,-105.5));
#6324=CARTESIAN_POINT('Ctrl Pts',(-6.46001186550229E-15,13.8750000027312,
-105.5));
#6325=CARTESIAN_POINT('Ctrl Pts',(43.6995308303615,13.8125000027312,-105.5));
#6326=CARTESIAN_POINT('Ctrl Pts',(74.5997654151808,13.7500000027312,-74.5997654151808));
#6327=CARTESIAN_POINT('Ctrl Pts',(105.5,13.6875000027312,-43.6995308303616));
#6328=CARTESIAN_POINT('Ctrl Pts',(105.5,13.6250000027312,-1.29200237310046E-14));
#6329=CARTESIAN_POINT('Ctrl Pts',(105.5,13.5625000027312,43.6995308303615));
#6330=CARTESIAN_POINT('Ctrl Pts',(74.5997654151808,13.5000000027312,74.5997654151808));
#6331=CARTESIAN_POINT('Ctrl Pts',(43.6995308303616,13.4375000027312,105.5));
#6332=CARTESIAN_POINT('Ctrl Pts',(1.93800355965069E-14,13.3750000027312,
105.5));
#6333=CARTESIAN_POINT('Origin',(0.,105.,0.));
#6334=CARTESIAN_POINT('',(3.23000593275114E-15,15.3750000027312,105.5));
#6335=CARTESIAN_POINT('',(3.23000593275114E-15,15.25,105.5));
#6336=CARTESIAN_POINT('',(-1.29200237310046E-14,105.,105.5));
#6337=CARTESIAN_POINT('Ctrl Pts',(1.93800355965069E-14,15.25,105.5));
#6338=CARTESIAN_POINT('Ctrl Pts',(-43.6995308303616,15.1875,105.5));
#6339=CARTESIAN_POINT('Ctrl Pts',(-74.5997654151808,15.125,74.5997654151808));
#6340=CARTESIAN_POINT('Ctrl Pts',(-105.5,15.0625,43.6995308303616));
#6341=CARTESIAN_POINT('Ctrl Pts',(-105.5,15.,0.));
#6342=CARTESIAN_POINT('Ctrl Pts',(-105.5,14.9375,-43.6995308303615));
#6343=CARTESIAN_POINT('Ctrl Pts',(-74.5997654151808,14.875,-74.5997654151808));
#6344=CARTESIAN_POINT('Ctrl Pts',(-43.6995308303615,14.8125,-105.5));
#6345=CARTESIAN_POINT('Ctrl Pts',(-6.46001186550229E-15,14.75,-105.5));
#6346=CARTESIAN_POINT('Ctrl Pts',(43.6995308303615,14.6875,-105.5));
#6347=CARTESIAN_POINT('Ctrl Pts',(74.5997654151808,14.625,-74.5997654151808));
#6348=CARTESIAN_POINT('Ctrl Pts',(105.5,14.5625,-43.6995308303616));
#6349=CARTESIAN_POINT('Ctrl Pts',(105.5,14.5,-1.29200237310046E-14));
#6350=CARTESIAN_POINT('Ctrl Pts',(105.5,14.4375,43.6995308303615));
#6351=CARTESIAN_POINT('Ctrl Pts',(74.5997654151808,14.375,74.5997654151808));
#6352=CARTESIAN_POINT('Ctrl Pts',(43.6995308303616,14.3125,105.5));
#6353=CARTESIAN_POINT('Ctrl Pts',(1.93800355965069E-14,14.25,105.5));
#6354=CARTESIAN_POINT('Ctrl Pts',(1.93800355965069E-14,15.3750000027312,
105.5));
#6355=CARTESIAN_POINT('Ctrl Pts',(-43.6995308303616,15.3125000027312,105.5));
#6356=CARTESIAN_POINT('Ctrl Pts',(-74.5997654151808,15.2500000027312,74.5997654151808));
#6357=CARTESIAN_POINT('Ctrl Pts',(-105.5,15.1875000027312,43.6995308303616));
#6358=CARTESIAN_POINT('Ctrl Pts',(-105.5,15.1250000027312,0.));
#6359=CARTESIAN_POINT('Ctrl Pts',(-105.5,15.0625000027312,-43.6995308303615));
#6360=CARTESIAN_POINT('Ctrl Pts',(-74.5997654151808,15.0000000027312,-74.5997654151808));
#6361=CARTESIAN_POINT('Ctrl Pts',(-43.6995308303615,14.9375000027312,-105.5));
#6362=CARTESIAN_POINT('Ctrl Pts',(-6.46001186550229E-15,14.8750000027312,
-105.5));
#6363=CARTESIAN_POINT('Ctrl Pts',(43.6995308303615,14.8125000027312,-105.5));
#6364=CARTESIAN_POINT('Ctrl Pts',(74.5997654151808,14.7500000027312,-74.5997654151808));
#6365=CARTESIAN_POINT('Ctrl Pts',(105.5,14.6875000027312,-43.6995308303616));
#6366=CARTESIAN_POINT('Ctrl Pts',(105.5,14.6250000027312,-1.29200237310046E-14));
#6367=CARTESIAN_POINT('Ctrl Pts',(105.5,14.5625000027312,43.6995308303615));
#6368=CARTESIAN_POINT('Ctrl Pts',(74.5997654151808,14.5000000027312,74.5997654151808));
#6369=CARTESIAN_POINT('Ctrl Pts',(43.6995308303616,14.4375000027312,105.5));
#6370=CARTESIAN_POINT('Ctrl Pts',(1.93800355965069E-14,14.3750000027312,
105.5));
#6371=CARTESIAN_POINT('Origin',(0.,105.,0.));
#6372=CARTESIAN_POINT('',(3.23000593275114E-15,16.3750000027312,105.5));
#6373=CARTESIAN_POINT('',(3.23000593275114E-15,16.25,105.5));
#6374=CARTESIAN_POINT('',(-1.29200237310046E-14,105.,105.5));
#6375=CARTESIAN_POINT('Ctrl Pts',(1.93800355965069E-14,16.25,105.5));
#6376=CARTESIAN_POINT('Ctrl Pts',(-43.6995308303616,16.1875,105.5));
#6377=CARTESIAN_POINT('Ctrl Pts',(-74.5997654151808,16.125,74.5997654151808));
#6378=CARTESIAN_POINT('Ctrl Pts',(-105.5,16.0625,43.6995308303616));
#6379=CARTESIAN_POINT('Ctrl Pts',(-105.5,16.,0.));
#6380=CARTESIAN_POINT('Ctrl Pts',(-105.5,15.9375,-43.6995308303615));
#6381=CARTESIAN_POINT('Ctrl Pts',(-74.5997654151808,15.875,-74.5997654151808));
#6382=CARTESIAN_POINT('Ctrl Pts',(-43.6995308303615,15.8125,-105.5));
#6383=CARTESIAN_POINT('Ctrl Pts',(-6.46001186550229E-15,15.75,-105.5));
#6384=CARTESIAN_POINT('Ctrl Pts',(43.6995308303615,15.6875,-105.5));
#6385=CARTESIAN_POINT('Ctrl Pts',(74.5997654151808,15.625,-74.5997654151808));
#6386=CARTESIAN_POINT('Ctrl Pts',(105.5,15.5625,-43.6995308303616));
#6387=CARTESIAN_POINT('Ctrl Pts',(105.5,15.5,-1.29200237310046E-14));
#6388=CARTESIAN_POINT('Ctrl Pts',(105.5,15.4375,43.6995308303615));
#6389=CARTESIAN_POINT('Ctrl Pts',(74.5997654151808,15.375,74.5997654151808));
#6390=CARTESIAN_POINT('Ctrl Pts',(43.6995308303616,15.3125,105.5));
#6391=CARTESIAN_POINT('Ctrl Pts',(1.93800355965069E-14,15.25,105.5));
#6392=CARTESIAN_POINT('Ctrl Pts',(1.93800355965069E-14,16.3750000027312,
105.5));
#6393=CARTESIAN_POINT('Ctrl Pts',(-43.6995308303616,16.3125000027312,105.5));
#6394=CARTESIAN_POINT('Ctrl Pts',(-74.5997654151808,16.2500000027312,74.5997654151808));
#6395=CARTESIAN_POINT('Ctrl Pts',(-105.5,16.1875000027312,43.6995308303616));
#6396=CARTESIAN_POINT('Ctrl Pts',(-105.5,16.1250000027312,0.));
#6397=CARTESIAN_POINT('Ctrl Pts',(-105.5,16.0625000027312,-43.6995308303615));
#6398=CARTESIAN_POINT('Ctrl Pts',(-74.5997654151808,16.0000000027312,-74.5997654151808));
#6399=CARTESIAN_POINT('Ctrl Pts',(-43.6995308303615,15.9375000027312,-105.5));
#6400=CARTESIAN_POINT('Ctrl Pts',(-6.46001186550229E-15,15.8750000027312,
-105.5));
#6401=CARTESIAN_POINT('Ctrl Pts',(43.6995308303615,15.8125000027312,-105.5));
#6402=CARTESIAN_POINT('Ctrl Pts',(74.5997654151808,15.7500000027312,-74.5997654151808));
#6403=CARTESIAN_POINT('Ctrl Pts',(105.5,15.6875000027312,-43.6995308303616));
#6404=CARTESIAN_POINT('Ctrl Pts',(105.5,15.6250000027312,-1.29200237310046E-14));
#6405=CARTESIAN_POINT('Ctrl Pts',(105.5,15.5625000027312,43.6995308303615));
#6406=CARTESIAN_POINT('Ctrl Pts',(74.5997654151808,15.5000000027312,74.5997654151808));
#6407=CARTESIAN_POINT('Ctrl Pts',(43.6995308303616,15.4375000027312,105.5));
#6408=CARTESIAN_POINT('Ctrl Pts',(1.93800355965069E-14,15.3750000027312,
105.5));
#6409=CARTESIAN_POINT('Origin',(0.,105.,0.));
#6410=CARTESIAN_POINT('',(3.23000593275114E-15,17.3750000027312,105.5));
#6411=CARTESIAN_POINT('',(3.23000593275114E-15,17.25,105.5));
#6412=CARTESIAN_POINT('',(-1.29200237310046E-14,105.,105.5));
#6413=CARTESIAN_POINT('Ctrl Pts',(1.93800355965069E-14,17.25,105.5));
#6414=CARTESIAN_POINT('Ctrl Pts',(-43.6995308303616,17.1875,105.5));
#6415=CARTESIAN_POINT('Ctrl Pts',(-74.5997654151808,17.125,74.5997654151808));
#6416=CARTESIAN_POINT('Ctrl Pts',(-105.5,17.0625,43.6995308303616));
#6417=CARTESIAN_POINT('Ctrl Pts',(-105.5,17.,0.));
#6418=CARTESIAN_POINT('Ctrl Pts',(-105.5,16.9375,-43.6995308303615));
#6419=CARTESIAN_POINT('Ctrl Pts',(-74.5997654151808,16.875,-74.5997654151808));
#6420=CARTESIAN_POINT('Ctrl Pts',(-43.6995308303615,16.8125,-105.5));
#6421=CARTESIAN_POINT('Ctrl Pts',(-6.46001186550229E-15,16.75,-105.5));
#6422=CARTESIAN_POINT('Ctrl Pts',(43.6995308303615,16.6875,-105.5));
#6423=CARTESIAN_POINT('Ctrl Pts',(74.5997654151808,16.625,-74.5997654151808));
#6424=CARTESIAN_POINT('Ctrl Pts',(105.5,16.5625,-43.6995308303616));
#6425=CARTESIAN_POINT('Ctrl Pts',(105.5,16.5,-1.29200237310046E-14));
#6426=CARTESIAN_POINT('Ctrl Pts',(105.5,16.4375,43.6995308303615));
#6427=CARTESIAN_POINT('Ctrl Pts',(74.5997654151808,16.375,74.5997654151808));
#6428=CARTESIAN_POINT('Ctrl Pts',(43.6995308303616,16.3125,105.5));
#6429=CARTESIAN_POINT('Ctrl Pts',(1.93800355965069E-14,16.25,105.5));
#6430=CARTESIAN_POINT('Ctrl Pts',(1.93800355965069E-14,17.3750000027312,
105.5));
#6431=CARTESIAN_POINT('Ctrl Pts',(-43.6995308303616,17.3125000027312,105.5));
#6432=CARTESIAN_POINT('Ctrl Pts',(-74.5997654151808,17.2500000027312,74.5997654151808));
#6433=CARTESIAN_POINT('Ctrl Pts',(-105.5,17.1875000027312,43.6995308303616));
#6434=CARTESIAN_POINT('Ctrl Pts',(-105.5,17.1250000027312,0.));
#6435=CARTESIAN_POINT('Ctrl Pts',(-105.5,17.0625000027312,-43.6995308303615));
#6436=CARTESIAN_POINT('Ctrl Pts',(-74.5997654151808,17.0000000027312,-74.5997654151808));
#6437=CARTESIAN_POINT('Ctrl Pts',(-43.6995308303615,16.9375000027312,-105.5));
#6438=CARTESIAN_POINT('Ctrl Pts',(-6.46001186550229E-15,16.8750000027312,
-105.5));
#6439=CARTESIAN_POINT('Ctrl Pts',(43.6995308303615,16.8125000027312,-105.5));
#6440=CARTESIAN_POINT('Ctrl Pts',(74.5997654151808,16.7500000027312,-74.5997654151808));
#6441=CARTESIAN_POINT('Ctrl Pts',(105.5,16.6875000027312,-43.6995308303616));
#6442=CARTESIAN_POINT('Ctrl Pts',(105.5,16.6250000027312,-1.29200237310046E-14));
#6443=CARTESIAN_POINT('Ctrl Pts',(105.5,16.5625000027312,43.6995308303615));
#6444=CARTESIAN_POINT('Ctrl Pts',(74.5997654151808,16.5000000027312,74.5997654151808));
#6445=CARTESIAN_POINT('Ctrl Pts',(43.6995308303616,16.4375000027312,105.5));
#6446=CARTESIAN_POINT('Ctrl Pts',(1.93800355965069E-14,16.3750000027312,
105.5));
#6447=CARTESIAN_POINT('Origin',(0.,105.,0.));
#6448=CARTESIAN_POINT('',(3.23000593275114E-15,18.3750000027312,105.5));
#6449=CARTESIAN_POINT('',(3.23000593275114E-15,18.25,105.5));
#6450=CARTESIAN_POINT('',(-1.29200237310046E-14,105.,105.5));
#6451=CARTESIAN_POINT('Ctrl Pts',(1.93800355965069E-14,18.25,105.5));
#6452=CARTESIAN_POINT('Ctrl Pts',(-43.6995308303616,18.1875,105.5));
#6453=CARTESIAN_POINT('Ctrl Pts',(-74.5997654151808,18.125,74.5997654151808));
#6454=CARTESIAN_POINT('Ctrl Pts',(-105.5,18.0625,43.6995308303616));
#6455=CARTESIAN_POINT('Ctrl Pts',(-105.5,18.,0.));
#6456=CARTESIAN_POINT('Ctrl Pts',(-105.5,17.9375,-43.6995308303615));
#6457=CARTESIAN_POINT('Ctrl Pts',(-74.5997654151808,17.875,-74.5997654151808));
#6458=CARTESIAN_POINT('Ctrl Pts',(-43.6995308303615,17.8125,-105.5));
#6459=CARTESIAN_POINT('Ctrl Pts',(-6.46001186550229E-15,17.75,-105.5));
#6460=CARTESIAN_POINT('Ctrl Pts',(43.6995308303615,17.6875,-105.5));
#6461=CARTESIAN_POINT('Ctrl Pts',(74.5997654151808,17.625,-74.5997654151808));
#6462=CARTESIAN_POINT('Ctrl Pts',(105.5,17.5625,-43.6995308303616));
#6463=CARTESIAN_POINT('Ctrl Pts',(105.5,17.5,-1.29200237310046E-14));
#6464=CARTESIAN_POINT('Ctrl Pts',(105.5,17.4375,43.6995308303615));
#6465=CARTESIAN_POINT('Ctrl Pts',(74.5997654151808,17.375,74.5997654151808));
#6466=CARTESIAN_POINT('Ctrl Pts',(43.6995308303616,17.3125,105.5));
#6467=CARTESIAN_POINT('Ctrl Pts',(1.93800355965069E-14,17.25,105.5));
#6468=CARTESIAN_POINT('Ctrl Pts',(1.93800355965069E-14,18.3750000027312,
105.5));
#6469=CARTESIAN_POINT('Ctrl Pts',(-43.6995308303616,18.3125000027312,105.5));
#6470=CARTESIAN_POINT('Ctrl Pts',(-74.5997654151808,18.2500000027312,74.5997654151808));
#6471=CARTESIAN_POINT('Ctrl Pts',(-105.5,18.1875000027312,43.6995308303616));
#6472=CARTESIAN_POINT('Ctrl Pts',(-105.5,18.1250000027312,0.));
#6473=CARTESIAN_POINT('Ctrl Pts',(-105.5,18.0625000027312,-43.6995308303615));
#6474=CARTESIAN_POINT('Ctrl Pts',(-74.5997654151808,18.0000000027312,-74.5997654151808));
#6475=CARTESIAN_POINT('Ctrl Pts',(-43.6995308303615,17.9375000027312,-105.5));
#6476=CARTESIAN_POINT('Ctrl Pts',(-6.46001186550229E-15,17.8750000027312,
-105.5));
#6477=CARTESIAN_POINT('Ctrl Pts',(43.6995308303615,17.8125000027312,-105.5));
#6478=CARTESIAN_POINT('Ctrl Pts',(74.5997654151808,17.7500000027312,-74.5997654151808));
#6479=CARTESIAN_POINT('Ctrl Pts',(105.5,17.6875000027312,-43.6995308303616));
#6480=CARTESIAN_POINT('Ctrl Pts',(105.5,17.6250000027312,-1.29200237310046E-14));
#6481=CARTESIAN_POINT('Ctrl Pts',(105.5,17.5625000027312,43.6995308303615));
#6482=CARTESIAN_POINT('Ctrl Pts',(74.5997654151808,17.5000000027312,74.5997654151808));
#6483=CARTESIAN_POINT('Ctrl Pts',(43.6995308303616,17.4375000027312,105.5));
#6484=CARTESIAN_POINT('Ctrl Pts',(1.93800355965069E-14,17.3750000027312,
105.5));
#6485=CARTESIAN_POINT('Origin',(0.,105.,0.));
#6486=CARTESIAN_POINT('',(3.23000593275114E-15,19.3750000027312,105.5));
#6487=CARTESIAN_POINT('',(3.23000593275114E-15,19.25,105.5));
#6488=CARTESIAN_POINT('',(-1.29200237310046E-14,105.,105.5));
#6489=CARTESIAN_POINT('Ctrl Pts',(1.93800355965069E-14,19.25,105.5));
#6490=CARTESIAN_POINT('Ctrl Pts',(-43.6995308303616,19.1875,105.5));
#6491=CARTESIAN_POINT('Ctrl Pts',(-74.5997654151808,19.125,74.5997654151808));
#6492=CARTESIAN_POINT('Ctrl Pts',(-105.5,19.0625,43.6995308303616));
#6493=CARTESIAN_POINT('Ctrl Pts',(-105.5,19.,0.));
#6494=CARTESIAN_POINT('Ctrl Pts',(-105.5,18.9375,-43.6995308303615));
#6495=CARTESIAN_POINT('Ctrl Pts',(-74.5997654151808,18.875,-74.5997654151808));
#6496=CARTESIAN_POINT('Ctrl Pts',(-43.6995308303615,18.8125,-105.5));
#6497=CARTESIAN_POINT('Ctrl Pts',(-6.46001186550229E-15,18.75,-105.5));
#6498=CARTESIAN_POINT('Ctrl Pts',(43.6995308303615,18.6875,-105.5));
#6499=CARTESIAN_POINT('Ctrl Pts',(74.5997654151808,18.625,-74.5997654151808));
#6500=CARTESIAN_POINT('Ctrl Pts',(105.5,18.5625,-43.6995308303616));
#6501=CARTESIAN_POINT('Ctrl Pts',(105.5,18.5,-1.29200237310046E-14));
#6502=CARTESIAN_POINT('Ctrl Pts',(105.5,18.4375,43.6995308303615));
#6503=CARTESIAN_POINT('Ctrl Pts',(74.5997654151808,18.375,74.5997654151808));
#6504=CARTESIAN_POINT('Ctrl Pts',(43.6995308303616,18.3125,105.5));
#6505=CARTESIAN_POINT('Ctrl Pts',(1.93800355965069E-14,18.25,105.5));
#6506=CARTESIAN_POINT('Ctrl Pts',(1.93800355965069E-14,19.3750000027312,
105.5));
#6507=CARTESIAN_POINT('Ctrl Pts',(-43.6995308303616,19.3125000027312,105.5));
#6508=CARTESIAN_POINT('Ctrl Pts',(-74.5997654151808,19.2500000027312,74.5997654151808));
#6509=CARTESIAN_POINT('Ctrl Pts',(-105.5,19.1875000027312,43.6995308303616));
#6510=CARTESIAN_POINT('Ctrl Pts',(-105.5,19.1250000027312,0.));
#6511=CARTESIAN_POINT('Ctrl Pts',(-105.5,19.0625000027312,-43.6995308303615));
#6512=CARTESIAN_POINT('Ctrl Pts',(-74.5997654151808,19.0000000027312,-74.5997654151808));
#6513=CARTESIAN_POINT('Ctrl Pts',(-43.6995308303615,18.9375000027312,-105.5));
#6514=CARTESIAN_POINT('Ctrl Pts',(-6.46001186550229E-15,18.8750000027312,
-105.5));
#6515=CARTESIAN_POINT('Ctrl Pts',(43.6995308303615,18.8125000027312,-105.5));
#6516=CARTESIAN_POINT('Ctrl Pts',(74.5997654151808,18.7500000027312,-74.5997654151808));
#6517=CARTESIAN_POINT('Ctrl Pts',(105.5,18.6875000027312,-43.6995308303616));
#6518=CARTESIAN_POINT('Ctrl Pts',(105.5,18.6250000027312,-1.29200237310046E-14));
#6519=CARTESIAN_POINT('Ctrl Pts',(105.5,18.5625000027312,43.6995308303615));
#6520=CARTESIAN_POINT('Ctrl Pts',(74.5997654151808,18.5000000027312,74.5997654151808));
#6521=CARTESIAN_POINT('Ctrl Pts',(43.6995308303616,18.4375000027312,105.5));
#6522=CARTESIAN_POINT('Ctrl Pts',(1.93800355965069E-14,18.3750000027312,
105.5));
#6523=CARTESIAN_POINT('Origin',(0.,105.,0.));
#6524=CARTESIAN_POINT('',(3.23000593275114E-15,20.3750000027312,105.5));
#6525=CARTESIAN_POINT('',(3.23000593275114E-15,20.25,105.5));
#6526=CARTESIAN_POINT('',(-1.29200237310046E-14,105.,105.5));
#6527=CARTESIAN_POINT('Ctrl Pts',(1.93800355965069E-14,20.25,105.5));
#6528=CARTESIAN_POINT('Ctrl Pts',(-43.6995308303616,20.1875,105.5));
#6529=CARTESIAN_POINT('Ctrl Pts',(-74.5997654151808,20.125,74.5997654151808));
#6530=CARTESIAN_POINT('Ctrl Pts',(-105.5,20.0625,43.6995308303616));
#6531=CARTESIAN_POINT('Ctrl Pts',(-105.5,20.,0.));
#6532=CARTESIAN_POINT('Ctrl Pts',(-105.5,19.9375,-43.6995308303615));
#6533=CARTESIAN_POINT('Ctrl Pts',(-74.5997654151808,19.875,-74.5997654151808));
#6534=CARTESIAN_POINT('Ctrl Pts',(-43.6995308303615,19.8125,-105.5));
#6535=CARTESIAN_POINT('Ctrl Pts',(-6.46001186550229E-15,19.75,-105.5));
#6536=CARTESIAN_POINT('Ctrl Pts',(43.6995308303615,19.6875,-105.5));
#6537=CARTESIAN_POINT('Ctrl Pts',(74.5997654151808,19.625,-74.5997654151808));
#6538=CARTESIAN_POINT('Ctrl Pts',(105.5,19.5625,-43.6995308303616));
#6539=CARTESIAN_POINT('Ctrl Pts',(105.5,19.5,-1.29200237310046E-14));
#6540=CARTESIAN_POINT('Ctrl Pts',(105.5,19.4375,43.6995308303615));
#6541=CARTESIAN_POINT('Ctrl Pts',(74.5997654151808,19.375,74.5997654151808));
#6542=CARTESIAN_POINT('Ctrl Pts',(43.6995308303616,19.3125,105.5));
#6543=CARTESIAN_POINT('Ctrl Pts',(1.93800355965069E-14,19.25,105.5));
#6544=CARTESIAN_POINT('Ctrl Pts',(1.93800355965069E-14,20.3750000027312,
105.5));
#6545=CARTESIAN_POINT('Ctrl Pts',(-43.6995308303616,20.3125000027312,105.5));
#6546=CARTESIAN_POINT('Ctrl Pts',(-74.5997654151808,20.2500000027312,74.5997654151808));
#6547=CARTESIAN_POINT('Ctrl Pts',(-105.5,20.1875000027312,43.6995308303616));
#6548=CARTESIAN_POINT('Ctrl Pts',(-105.5,20.1250000027312,0.));
#6549=CARTESIAN_POINT('Ctrl Pts',(-105.5,20.0625000027312,-43.6995308303615));
#6550=CARTESIAN_POINT('Ctrl Pts',(-74.5997654151808,20.0000000027312,-74.5997654151808));
#6551=CARTESIAN_POINT('Ctrl Pts',(-43.6995308303615,19.9375000027312,-105.5));
#6552=CARTESIAN_POINT('Ctrl Pts',(-6.46001186550229E-15,19.8750000027312,
-105.5));
#6553=CARTESIAN_POINT('Ctrl Pts',(43.6995308303615,19.8125000027312,-105.5));
#6554=CARTESIAN_POINT('Ctrl Pts',(74.5997654151808,19.7500000027312,-74.5997654151808));
#6555=CARTESIAN_POINT('Ctrl Pts',(105.5,19.6875000027312,-43.6995308303616));
#6556=CARTESIAN_POINT('Ctrl Pts',(105.5,19.6250000027312,-1.29200237310046E-14));
#6557=CARTESIAN_POINT('Ctrl Pts',(105.5,19.5625000027312,43.6995308303615));
#6558=CARTESIAN_POINT('Ctrl Pts',(74.5997654151808,19.5000000027312,74.5997654151808));
#6559=CARTESIAN_POINT('Ctrl Pts',(43.6995308303616,19.4375000027312,105.5));
#6560=CARTESIAN_POINT('Ctrl Pts',(1.93800355965069E-14,19.3750000027312,
105.5));
#6561=CARTESIAN_POINT('Origin',(0.,105.,0.));
#6562=CARTESIAN_POINT('',(3.23000593275114E-15,21.3750000027312,105.5));
#6563=CARTESIAN_POINT('',(3.23000593275114E-15,21.25,105.5));
#6564=CARTESIAN_POINT('',(-1.29200237310046E-14,105.,105.5));
#6565=CARTESIAN_POINT('Ctrl Pts',(1.93800355965069E-14,21.25,105.5));
#6566=CARTESIAN_POINT('Ctrl Pts',(-43.6995308303616,21.1875,105.5));
#6567=CARTESIAN_POINT('Ctrl Pts',(-74.5997654151808,21.125,74.5997654151808));
#6568=CARTESIAN_POINT('Ctrl Pts',(-105.5,21.0625,43.6995308303616));
#6569=CARTESIAN_POINT('Ctrl Pts',(-105.5,21.,0.));
#6570=CARTESIAN_POINT('Ctrl Pts',(-105.5,20.9375,-43.6995308303615));
#6571=CARTESIAN_POINT('Ctrl Pts',(-74.5997654151808,20.875,-74.5997654151808));
#6572=CARTESIAN_POINT('Ctrl Pts',(-43.6995308303615,20.8125,-105.5));
#6573=CARTESIAN_POINT('Ctrl Pts',(-6.46001186550229E-15,20.75,-105.5));
#6574=CARTESIAN_POINT('Ctrl Pts',(43.6995308303615,20.6875,-105.5));
#6575=CARTESIAN_POINT('Ctrl Pts',(74.5997654151808,20.625,-74.5997654151808));
#6576=CARTESIAN_POINT('Ctrl Pts',(105.5,20.5625,-43.6995308303616));
#6577=CARTESIAN_POINT('Ctrl Pts',(105.5,20.5,-1.29200237310046E-14));
#6578=CARTESIAN_POINT('Ctrl Pts',(105.5,20.4375,43.6995308303615));
#6579=CARTESIAN_POINT('Ctrl Pts',(74.5997654151808,20.375,74.5997654151808));
#6580=CARTESIAN_POINT('Ctrl Pts',(43.6995308303616,20.3125,105.5));
#6581=CARTESIAN_POINT('Ctrl Pts',(1.93800355965069E-14,20.25,105.5));
#6582=CARTESIAN_POINT('Ctrl Pts',(1.93800355965069E-14,21.3750000027312,
105.5));
#6583=CARTESIAN_POINT('Ctrl Pts',(-43.6995308303616,21.3125000027312,105.5));
#6584=CARTESIAN_POINT('Ctrl Pts',(-74.5997654151808,21.2500000027312,74.5997654151808));
#6585=CARTESIAN_POINT('Ctrl Pts',(-105.5,21.1875000027312,43.6995308303616));
#6586=CARTESIAN_POINT('Ctrl Pts',(-105.5,21.1250000027312,0.));
#6587=CARTESIAN_POINT('Ctrl Pts',(-105.5,21.0625000027312,-43.6995308303615));
#6588=CARTESIAN_POINT('Ctrl Pts',(-74.5997654151808,21.0000000027312,-74.5997654151808));
#6589=CARTESIAN_POINT('Ctrl Pts',(-43.6995308303615,20.9375000027312,-105.5));
#6590=CARTESIAN_POINT('Ctrl Pts',(-6.46001186550229E-15,20.8750000027312,
-105.5));
#6591=CARTESIAN_POINT('Ctrl Pts',(43.6995308303615,20.8125000027312,-105.5));
#6592=CARTESIAN_POINT('Ctrl Pts',(74.5997654151808,20.7500000027312,-74.5997654151808));
#6593=CARTESIAN_POINT('Ctrl Pts',(105.5,20.6875000027312,-43.6995308303616));
#6594=CARTESIAN_POINT('Ctrl Pts',(105.5,20.6250000027312,-1.29200237310046E-14));
#6595=CARTESIAN_POINT('Ctrl Pts',(105.5,20.5625000027312,43.6995308303615));
#6596=CARTESIAN_POINT('Ctrl Pts',(74.5997654151808,20.5000000027312,74.5997654151808));
#6597=CARTESIAN_POINT('Ctrl Pts',(43.6995308303616,20.4375000027312,105.5));
#6598=CARTESIAN_POINT('Ctrl Pts',(1.93800355965069E-14,20.3750000027312,
105.5));
#6599=CARTESIAN_POINT('Origin',(0.,105.,0.));
#6600=CARTESIAN_POINT('',(3.23000593275114E-15,22.3750000027312,105.5));
#6601=CARTESIAN_POINT('',(3.23000593275114E-15,22.25,105.5));
#6602=CARTESIAN_POINT('',(-1.29200237310046E-14,105.,105.5));
#6603=CARTESIAN_POINT('Ctrl Pts',(1.93800355965069E-14,22.25,105.5));
#6604=CARTESIAN_POINT('Ctrl Pts',(-43.6995308303616,22.1875,105.5));
#6605=CARTESIAN_POINT('Ctrl Pts',(-74.5997654151808,22.125,74.5997654151808));
#6606=CARTESIAN_POINT('Ctrl Pts',(-105.5,22.0625,43.6995308303616));
#6607=CARTESIAN_POINT('Ctrl Pts',(-105.5,22.,0.));
#6608=CARTESIAN_POINT('Ctrl Pts',(-105.5,21.9375,-43.6995308303615));
#6609=CARTESIAN_POINT('Ctrl Pts',(-74.5997654151808,21.875,-74.5997654151808));
#6610=CARTESIAN_POINT('Ctrl Pts',(-43.6995308303615,21.8125,-105.5));
#6611=CARTESIAN_POINT('Ctrl Pts',(-6.46001186550229E-15,21.75,-105.5));
#6612=CARTESIAN_POINT('Ctrl Pts',(43.6995308303615,21.6875,-105.5));
#6613=CARTESIAN_POINT('Ctrl Pts',(74.5997654151808,21.625,-74.5997654151808));
#6614=CARTESIAN_POINT('Ctrl Pts',(105.5,21.5625,-43.6995308303616));
#6615=CARTESIAN_POINT('Ctrl Pts',(105.5,21.5,-1.29200237310046E-14));
#6616=CARTESIAN_POINT('Ctrl Pts',(105.5,21.4375,43.6995308303615));
#6617=CARTESIAN_POINT('Ctrl Pts',(74.5997654151808,21.375,74.5997654151808));
#6618=CARTESIAN_POINT('Ctrl Pts',(43.6995308303616,21.3125,105.5));
#6619=CARTESIAN_POINT('Ctrl Pts',(1.93800355965069E-14,21.25,105.5));
#6620=CARTESIAN_POINT('Ctrl Pts',(1.93800355965069E-14,22.3750000027312,
105.5));
#6621=CARTESIAN_POINT('Ctrl Pts',(-43.6995308303616,22.3125000027312,105.5));
#6622=CARTESIAN_POINT('Ctrl Pts',(-74.5997654151808,22.2500000027312,74.5997654151808));
#6623=CARTESIAN_POINT('Ctrl Pts',(-105.5,22.1875000027312,43.6995308303616));
#6624=CARTESIAN_POINT('Ctrl Pts',(-105.5,22.1250000027312,0.));
#6625=CARTESIAN_POINT('Ctrl Pts',(-105.5,22.0625000027312,-43.6995308303615));
#6626=CARTESIAN_POINT('Ctrl Pts',(-74.5997654151808,22.0000000027312,-74.5997654151808));
#6627=CARTESIAN_POINT('Ctrl Pts',(-43.6995308303615,21.9375000027312,-105.5));
#6628=CARTESIAN_POINT('Ctrl Pts',(-6.46001186550229E-15,21.8750000027312,
-105.5));
#6629=CARTESIAN_POINT('Ctrl Pts',(43.6995308303615,21.8125000027312,-105.5));
#6630=CARTESIAN_POINT('Ctrl Pts',(74.5997654151808,21.7500000027312,-74.5997654151808));
#6631=CARTESIAN_POINT('Ctrl Pts',(105.5,21.6875000027312,-43.6995308303616));
#6632=CARTESIAN_POINT('Ctrl Pts',(105.5,21.6250000027312,-1.29200237310046E-14));
#6633=CARTESIAN_POINT('Ctrl Pts',(105.5,21.5625000027312,43.6995308303615));
#6634=CARTESIAN_POINT('Ctrl Pts',(74.5997654151808,21.5000000027312,74.5997654151808));
#6635=CARTESIAN_POINT('Ctrl Pts',(43.6995308303616,21.4375000027312,105.5));
#6636=CARTESIAN_POINT('Ctrl Pts',(1.93800355965069E-14,21.3750000027312,
105.5));
#6637=CARTESIAN_POINT('Origin',(0.,105.,0.));
#6638=CARTESIAN_POINT('',(3.23000593275114E-15,23.3750000027312,105.5));
#6639=CARTESIAN_POINT('',(3.23000593275114E-15,23.25,105.5));
#6640=CARTESIAN_POINT('',(-1.29200237310046E-14,105.,105.5));
#6641=CARTESIAN_POINT('Ctrl Pts',(1.93800355965069E-14,23.25,105.5));
#6642=CARTESIAN_POINT('Ctrl Pts',(-43.6995308303616,23.1875,105.5));
#6643=CARTESIAN_POINT('Ctrl Pts',(-74.5997654151808,23.125,74.5997654151808));
#6644=CARTESIAN_POINT('Ctrl Pts',(-105.5,23.0625,43.6995308303616));
#6645=CARTESIAN_POINT('Ctrl Pts',(-105.5,23.,0.));
#6646=CARTESIAN_POINT('Ctrl Pts',(-105.5,22.9375,-43.6995308303615));
#6647=CARTESIAN_POINT('Ctrl Pts',(-74.5997654151808,22.875,-74.5997654151808));
#6648=CARTESIAN_POINT('Ctrl Pts',(-43.6995308303615,22.8125,-105.5));
#6649=CARTESIAN_POINT('Ctrl Pts',(-6.46001186550229E-15,22.75,-105.5));
#6650=CARTESIAN_POINT('Ctrl Pts',(43.6995308303615,22.6875,-105.5));
#6651=CARTESIAN_POINT('Ctrl Pts',(74.5997654151808,22.625,-74.5997654151808));
#6652=CARTESIAN_POINT('Ctrl Pts',(105.5,22.5625,-43.6995308303616));
#6653=CARTESIAN_POINT('Ctrl Pts',(105.5,22.5,-1.29200237310046E-14));
#6654=CARTESIAN_POINT('Ctrl Pts',(105.5,22.4375,43.6995308303615));
#6655=CARTESIAN_POINT('Ctrl Pts',(74.5997654151808,22.375,74.5997654151808));
#6656=CARTESIAN_POINT('Ctrl Pts',(43.6995308303616,22.3125,105.5));
#6657=CARTESIAN_POINT('Ctrl Pts',(1.93800355965069E-14,22.25,105.5));
#6658=CARTESIAN_POINT('Ctrl Pts',(1.93800355965069E-14,23.3750000027312,
105.5));
#6659=CARTESIAN_POINT('Ctrl Pts',(-43.6995308303616,23.3125000027312,105.5));
#6660=CARTESIAN_POINT('Ctrl Pts',(-74.5997654151808,23.2500000027312,74.5997654151808));
#6661=CARTESIAN_POINT('Ctrl Pts',(-105.5,23.1875000027312,43.6995308303616));
#6662=CARTESIAN_POINT('Ctrl Pts',(-105.5,23.1250000027312,0.));
#6663=CARTESIAN_POINT('Ctrl Pts',(-105.5,23.0625000027312,-43.6995308303615));
#6664=CARTESIAN_POINT('Ctrl Pts',(-74.5997654151808,23.0000000027312,-74.5997654151808));
#6665=CARTESIAN_POINT('Ctrl Pts',(-43.6995308303615,22.9375000027312,-105.5));
#6666=CARTESIAN_POINT('Ctrl Pts',(-6.46001186550229E-15,22.8750000027312,
-105.5));
#6667=CARTESIAN_POINT('Ctrl Pts',(43.6995308303615,22.8125000027312,-105.5));
#6668=CARTESIAN_POINT('Ctrl Pts',(74.5997654151808,22.7500000027312,-74.5997654151808));
#6669=CARTESIAN_POINT('Ctrl Pts',(105.5,22.6875000027312,-43.6995308303616));
#6670=CARTESIAN_POINT('Ctrl Pts',(105.5,22.6250000027312,-1.29200237310046E-14));
#6671=CARTESIAN_POINT('Ctrl Pts',(105.5,22.5625000027312,43.6995308303615));
#6672=CARTESIAN_POINT('Ctrl Pts',(74.5997654151808,22.5000000027312,74.5997654151808));
#6673=CARTESIAN_POINT('Ctrl Pts',(43.6995308303616,22.4375000027312,105.5));
#6674=CARTESIAN_POINT('Ctrl Pts',(1.93800355965069E-14,22.3750000027312,
105.5));
#6675=CARTESIAN_POINT('Origin',(0.,105.,0.));
#6676=CARTESIAN_POINT('',(3.23000593275114E-15,24.3750000027312,105.5));
#6677=CARTESIAN_POINT('',(3.23000593275114E-15,24.25,105.5));
#6678=CARTESIAN_POINT('',(-1.29200237310046E-14,105.,105.5));
#6679=CARTESIAN_POINT('Ctrl Pts',(1.93800355965069E-14,24.25,105.5));
#6680=CARTESIAN_POINT('Ctrl Pts',(-43.6995308303616,24.1875,105.5));
#6681=CARTESIAN_POINT('Ctrl Pts',(-74.5997654151808,24.125,74.5997654151808));
#6682=CARTESIAN_POINT('Ctrl Pts',(-105.5,24.0625,43.6995308303616));
#6683=CARTESIAN_POINT('Ctrl Pts',(-105.5,24.,0.));
#6684=CARTESIAN_POINT('Ctrl Pts',(-105.5,23.9375,-43.6995308303615));
#6685=CARTESIAN_POINT('Ctrl Pts',(-74.5997654151808,23.875,-74.5997654151808));
#6686=CARTESIAN_POINT('Ctrl Pts',(-43.6995308303615,23.8125,-105.5));
#6687=CARTESIAN_POINT('Ctrl Pts',(-6.46001186550229E-15,23.75,-105.5));
#6688=CARTESIAN_POINT('Ctrl Pts',(43.6995308303615,23.6875,-105.5));
#6689=CARTESIAN_POINT('Ctrl Pts',(74.5997654151808,23.625,-74.5997654151808));
#6690=CARTESIAN_POINT('Ctrl Pts',(105.5,23.5625,-43.6995308303616));
#6691=CARTESIAN_POINT('Ctrl Pts',(105.5,23.5,-1.29200237310046E-14));
#6692=CARTESIAN_POINT('Ctrl Pts',(105.5,23.4375,43.6995308303615));
#6693=CARTESIAN_POINT('Ctrl Pts',(74.5997654151808,23.375,74.5997654151808));
#6694=CARTESIAN_POINT('Ctrl Pts',(43.6995308303616,23.3125,105.5));
#6695=CARTESIAN_POINT('Ctrl Pts',(1.93800355965069E-14,23.25,105.5));
#6696=CARTESIAN_POINT('Ctrl Pts',(1.93800355965069E-14,24.3750000027312,
105.5));
#6697=CARTESIAN_POINT('Ctrl Pts',(-43.6995308303616,24.3125000027312,105.5));
#6698=CARTESIAN_POINT('Ctrl Pts',(-74.5997654151808,24.2500000027312,74.5997654151808));
#6699=CARTESIAN_POINT('Ctrl Pts',(-105.5,24.1875000027312,43.6995308303616));
#6700=CARTESIAN_POINT('Ctrl Pts',(-105.5,24.1250000027312,0.));
#6701=CARTESIAN_POINT('Ctrl Pts',(-105.5,24.0625000027312,-43.6995308303615));
#6702=CARTESIAN_POINT('Ctrl Pts',(-74.5997654151808,24.0000000027312,-74.5997654151808));
#6703=CARTESIAN_POINT('Ctrl Pts',(-43.6995308303615,23.9375000027312,-105.5));
#6704=CARTESIAN_POINT('Ctrl Pts',(-6.46001186550229E-15,23.8750000027312,
-105.5));
#6705=CARTESIAN_POINT('Ctrl Pts',(43.6995308303615,23.8125000027312,-105.5));
#6706=CARTESIAN_POINT('Ctrl Pts',(74.5997654151808,23.7500000027312,-74.5997654151808));
#6707=CARTESIAN_POINT('Ctrl Pts',(105.5,23.6875000027312,-43.6995308303616));
#6708=CARTESIAN_POINT('Ctrl Pts',(105.5,23.6250000027312,-1.29200237310046E-14));
#6709=CARTESIAN_POINT('Ctrl Pts',(105.5,23.5625000027312,43.6995308303615));
#6710=CARTESIAN_POINT('Ctrl Pts',(74.5997654151808,23.5000000027312,74.5997654151808));
#6711=CARTESIAN_POINT('Ctrl Pts',(43.6995308303616,23.4375000027312,105.5));
#6712=CARTESIAN_POINT('Ctrl Pts',(1.93800355965069E-14,23.3750000027312,
105.5));
#6713=CARTESIAN_POINT('Origin',(0.,105.,0.));
#6714=CARTESIAN_POINT('',(3.23000593275114E-15,25.3750000027312,105.5));
#6715=CARTESIAN_POINT('',(3.23000593275114E-15,25.25,105.5));
#6716=CARTESIAN_POINT('',(-1.29200237310046E-14,105.,105.5));
#6717=CARTESIAN_POINT('Ctrl Pts',(1.93800355965069E-14,25.25,105.5));
#6718=CARTESIAN_POINT('Ctrl Pts',(-43.6995308303616,25.1875,105.5));
#6719=CARTESIAN_POINT('Ctrl Pts',(-74.5997654151808,25.125,74.5997654151808));
#6720=CARTESIAN_POINT('Ctrl Pts',(-105.5,25.0625,43.6995308303616));
#6721=CARTESIAN_POINT('Ctrl Pts',(-105.5,25.,0.));
#6722=CARTESIAN_POINT('Ctrl Pts',(-105.5,24.9375,-43.6995308303615));
#6723=CARTESIAN_POINT('Ctrl Pts',(-74.5997654151808,24.875,-74.5997654151808));
#6724=CARTESIAN_POINT('Ctrl Pts',(-43.6995308303615,24.8125,-105.5));
#6725=CARTESIAN_POINT('Ctrl Pts',(-6.46001186550229E-15,24.75,-105.5));
#6726=CARTESIAN_POINT('Ctrl Pts',(43.6995308303615,24.6875,-105.5));
#6727=CARTESIAN_POINT('Ctrl Pts',(74.5997654151808,24.625,-74.5997654151808));
#6728=CARTESIAN_POINT('Ctrl Pts',(105.5,24.5625,-43.6995308303616));
#6729=CARTESIAN_POINT('Ctrl Pts',(105.5,24.5,-1.29200237310046E-14));
#6730=CARTESIAN_POINT('Ctrl Pts',(105.5,24.4375,43.6995308303615));
#6731=CARTESIAN_POINT('Ctrl Pts',(74.5997654151808,24.375,74.5997654151808));
#6732=CARTESIAN_POINT('Ctrl Pts',(43.6995308303616,24.3125,105.5));
#6733=CARTESIAN_POINT('Ctrl Pts',(1.93800355965069E-14,24.25,105.5));
#6734=CARTESIAN_POINT('Ctrl Pts',(1.93800355965069E-14,25.3750000027312,
105.5));
#6735=CARTESIAN_POINT('Ctrl Pts',(-43.6995308303616,25.3125000027312,105.5));
#6736=CARTESIAN_POINT('Ctrl Pts',(-74.5997654151808,25.2500000027312,74.5997654151808));
#6737=CARTESIAN_POINT('Ctrl Pts',(-105.5,25.1875000027312,43.6995308303616));
#6738=CARTESIAN_POINT('Ctrl Pts',(-105.5,25.1250000027312,0.));
#6739=CARTESIAN_POINT('Ctrl Pts',(-105.5,25.0625000027312,-43.6995308303615));
#6740=CARTESIAN_POINT('Ctrl Pts',(-74.5997654151808,25.0000000027312,-74.5997654151808));
#6741=CARTESIAN_POINT('Ctrl Pts',(-43.6995308303615,24.9375000027312,-105.5));
#6742=CARTESIAN_POINT('Ctrl Pts',(-6.46001186550229E-15,24.8750000027312,
-105.5));
#6743=CARTESIAN_POINT('Ctrl Pts',(43.6995308303615,24.8125000027312,-105.5));
#6744=CARTESIAN_POINT('Ctrl Pts',(74.5997654151808,24.7500000027312,-74.5997654151808));
#6745=CARTESIAN_POINT('Ctrl Pts',(105.5,24.6875000027312,-43.6995308303616));
#6746=CARTESIAN_POINT('Ctrl Pts',(105.5,24.6250000027312,-1.29200237310046E-14));
#6747=CARTESIAN_POINT('Ctrl Pts',(105.5,24.5625000027312,43.6995308303615));
#6748=CARTESIAN_POINT('Ctrl Pts',(74.5997654151808,24.5000000027312,74.5997654151808));
#6749=CARTESIAN_POINT('Ctrl Pts',(43.6995308303616,24.4375000027312,105.5));
#6750=CARTESIAN_POINT('Ctrl Pts',(1.93800355965069E-14,24.3750000027312,
105.5));
#6751=CARTESIAN_POINT('Origin',(0.,105.,0.));
#6752=CARTESIAN_POINT('',(3.23000593275114E-15,26.3750000027312,105.5));
#6753=CARTESIAN_POINT('',(3.23000593275114E-15,26.25,105.5));
#6754=CARTESIAN_POINT('',(-1.29200237310046E-14,105.,105.5));
#6755=CARTESIAN_POINT('Ctrl Pts',(1.93800355965069E-14,26.25,105.5));
#6756=CARTESIAN_POINT('Ctrl Pts',(-43.6995308303616,26.1875,105.5));
#6757=CARTESIAN_POINT('Ctrl Pts',(-74.5997654151808,26.125,74.5997654151808));
#6758=CARTESIAN_POINT('Ctrl Pts',(-105.5,26.0625,43.6995308303616));
#6759=CARTESIAN_POINT('Ctrl Pts',(-105.5,26.,0.));
#6760=CARTESIAN_POINT('Ctrl Pts',(-105.5,25.9375,-43.6995308303615));
#6761=CARTESIAN_POINT('Ctrl Pts',(-74.5997654151808,25.875,-74.5997654151808));
#6762=CARTESIAN_POINT('Ctrl Pts',(-43.6995308303615,25.8125,-105.5));
#6763=CARTESIAN_POINT('Ctrl Pts',(-6.46001186550229E-15,25.75,-105.5));
#6764=CARTESIAN_POINT('Ctrl Pts',(43.6995308303615,25.6875,-105.5));
#6765=CARTESIAN_POINT('Ctrl Pts',(74.5997654151808,25.625,-74.5997654151808));
#6766=CARTESIAN_POINT('Ctrl Pts',(105.5,25.5625,-43.6995308303616));
#6767=CARTESIAN_POINT('Ctrl Pts',(105.5,25.5,-1.29200237310046E-14));
#6768=CARTESIAN_POINT('Ctrl Pts',(105.5,25.4375,43.6995308303615));
#6769=CARTESIAN_POINT('Ctrl Pts',(74.5997654151808,25.375,74.5997654151808));
#6770=CARTESIAN_POINT('Ctrl Pts',(43.6995308303616,25.3125,105.5));
#6771=CARTESIAN_POINT('Ctrl Pts',(1.93800355965069E-14,25.25,105.5));
#6772=CARTESIAN_POINT('Ctrl Pts',(1.93800355965069E-14,26.3750000027312,
105.5));
#6773=CARTESIAN_POINT('Ctrl Pts',(-43.6995308303616,26.3125000027312,105.5));
#6774=CARTESIAN_POINT('Ctrl Pts',(-74.5997654151808,26.2500000027312,74.5997654151808));
#6775=CARTESIAN_POINT('Ctrl Pts',(-105.5,26.1875000027312,43.6995308303616));
#6776=CARTESIAN_POINT('Ctrl Pts',(-105.5,26.1250000027312,0.));
#6777=CARTESIAN_POINT('Ctrl Pts',(-105.5,26.0625000027312,-43.6995308303615));
#6778=CARTESIAN_POINT('Ctrl Pts',(-74.5997654151808,26.0000000027312,-74.5997654151808));
#6779=CARTESIAN_POINT('Ctrl Pts',(-43.6995308303615,25.9375000027312,-105.5));
#6780=CARTESIAN_POINT('Ctrl Pts',(-6.46001186550229E-15,25.8750000027312,
-105.5));
#6781=CARTESIAN_POINT('Ctrl Pts',(43.6995308303615,25.8125000027312,-105.5));
#6782=CARTESIAN_POINT('Ctrl Pts',(74.5997654151808,25.7500000027312,-74.5997654151808));
#6783=CARTESIAN_POINT('Ctrl Pts',(105.5,25.6875000027312,-43.6995308303616));
#6784=CARTESIAN_POINT('Ctrl Pts',(105.5,25.6250000027312,-1.29200237310046E-14));
#6785=CARTESIAN_POINT('Ctrl Pts',(105.5,25.5625000027312,43.6995308303615));
#6786=CARTESIAN_POINT('Ctrl Pts',(74.5997654151808,25.5000000027312,74.5997654151808));
#6787=CARTESIAN_POINT('Ctrl Pts',(43.6995308303616,25.4375000027312,105.5));
#6788=CARTESIAN_POINT('Ctrl Pts',(1.93800355965069E-14,25.3750000027312,
105.5));
#6789=CARTESIAN_POINT('Origin',(0.,105.,0.));
#6790=CARTESIAN_POINT('',(3.23000593275114E-15,27.3750000027312,105.5));
#6791=CARTESIAN_POINT('',(3.23000593275114E-15,27.25,105.5));
#6792=CARTESIAN_POINT('',(-1.29200237310046E-14,105.,105.5));
#6793=CARTESIAN_POINT('Ctrl Pts',(1.93800355965069E-14,27.25,105.5));
#6794=CARTESIAN_POINT('Ctrl Pts',(-43.6995308303616,27.1875,105.5));
#6795=CARTESIAN_POINT('Ctrl Pts',(-74.5997654151808,27.125,74.5997654151808));
#6796=CARTESIAN_POINT('Ctrl Pts',(-105.5,27.0625,43.6995308303616));
#6797=CARTESIAN_POINT('Ctrl Pts',(-105.5,27.,0.));
#6798=CARTESIAN_POINT('Ctrl Pts',(-105.5,26.9375,-43.6995308303615));
#6799=CARTESIAN_POINT('Ctrl Pts',(-74.5997654151808,26.875,-74.5997654151808));
#6800=CARTESIAN_POINT('Ctrl Pts',(-43.6995308303615,26.8125,-105.5));
#6801=CARTESIAN_POINT('Ctrl Pts',(-6.46001186550229E-15,26.75,-105.5));
#6802=CARTESIAN_POINT('Ctrl Pts',(43.6995308303615,26.6875,-105.5));
#6803=CARTESIAN_POINT('Ctrl Pts',(74.5997654151808,26.625,-74.5997654151808));
#6804=CARTESIAN_POINT('Ctrl Pts',(105.5,26.5625,-43.6995308303616));
#6805=CARTESIAN_POINT('Ctrl Pts',(105.5,26.5,-1.29200237310046E-14));
#6806=CARTESIAN_POINT('Ctrl Pts',(105.5,26.4375,43.6995308303615));
#6807=CARTESIAN_POINT('Ctrl Pts',(74.5997654151808,26.375,74.5997654151808));
#6808=CARTESIAN_POINT('Ctrl Pts',(43.6995308303616,26.3125,105.5));
#6809=CARTESIAN_POINT('Ctrl Pts',(1.93800355965069E-14,26.25,105.5));
#6810=CARTESIAN_POINT('Ctrl Pts',(1.93800355965069E-14,27.3750000027312,
105.5));
#6811=CARTESIAN_POINT('Ctrl Pts',(-43.6995308303616,27.3125000027312,105.5));
#6812=CARTESIAN_POINT('Ctrl Pts',(-74.5997654151808,27.2500000027312,74.5997654151808));
#6813=CARTESIAN_POINT('Ctrl Pts',(-105.5,27.1875000027312,43.6995308303616));
#6814=CARTESIAN_POINT('Ctrl Pts',(-105.5,27.1250000027312,0.));
#6815=CARTESIAN_POINT('Ctrl Pts',(-105.5,27.0625000027312,-43.6995308303615));
#6816=CARTESIAN_POINT('Ctrl Pts',(-74.5997654151808,27.0000000027312,-74.5997654151808));
#6817=CARTESIAN_POINT('Ctrl Pts',(-43.6995308303615,26.9375000027312,-105.5));
#6818=CARTESIAN_POINT('Ctrl Pts',(-6.46001186550229E-15,26.8750000027312,
-105.5));
#6819=CARTESIAN_POINT('Ctrl Pts',(43.6995308303615,26.8125000027312,-105.5));
#6820=CARTESIAN_POINT('Ctrl Pts',(74.5997654151808,26.7500000027312,-74.5997654151808));
#6821=CARTESIAN_POINT('Ctrl Pts',(105.5,26.6875000027312,-43.6995308303616));
#6822=CARTESIAN_POINT('Ctrl Pts',(105.5,26.6250000027312,-1.29200237310046E-14));
#6823=CARTESIAN_POINT('Ctrl Pts',(105.5,26.5625000027312,43.6995308303615));
#6824=CARTESIAN_POINT('Ctrl Pts',(74.5997654151808,26.5000000027312,74.5997654151808));
#6825=CARTESIAN_POINT('Ctrl Pts',(43.6995308303616,26.4375000027312,105.5));
#6826=CARTESIAN_POINT('Ctrl Pts',(1.93800355965069E-14,26.3750000027312,
105.5));
#6827=CARTESIAN_POINT('Origin',(0.,105.,0.));
#6828=CARTESIAN_POINT('',(3.23000593275114E-15,28.3750000027312,105.5));
#6829=CARTESIAN_POINT('',(3.23000593275114E-15,28.25,105.5));
#6830=CARTESIAN_POINT('',(-1.29200237310046E-14,105.,105.5));
#6831=CARTESIAN_POINT('Ctrl Pts',(1.93800355965069E-14,28.25,105.5));
#6832=CARTESIAN_POINT('Ctrl Pts',(-43.6995308303616,28.1875,105.5));
#6833=CARTESIAN_POINT('Ctrl Pts',(-74.5997654151808,28.125,74.5997654151808));
#6834=CARTESIAN_POINT('Ctrl Pts',(-105.5,28.0625,43.6995308303616));
#6835=CARTESIAN_POINT('Ctrl Pts',(-105.5,28.,0.));
#6836=CARTESIAN_POINT('Ctrl Pts',(-105.5,27.9375,-43.6995308303615));
#6837=CARTESIAN_POINT('Ctrl Pts',(-74.5997654151808,27.875,-74.5997654151808));
#6838=CARTESIAN_POINT('Ctrl Pts',(-43.6995308303615,27.8125,-105.5));
#6839=CARTESIAN_POINT('Ctrl Pts',(-6.46001186550229E-15,27.75,-105.5));
#6840=CARTESIAN_POINT('Ctrl Pts',(43.6995308303615,27.6875,-105.5));
#6841=CARTESIAN_POINT('Ctrl Pts',(74.5997654151808,27.625,-74.5997654151808));
#6842=CARTESIAN_POINT('Ctrl Pts',(105.5,27.5625,-43.6995308303616));
#6843=CARTESIAN_POINT('Ctrl Pts',(105.5,27.5,-1.29200237310046E-14));
#6844=CARTESIAN_POINT('Ctrl Pts',(105.5,27.4375,43.6995308303615));
#6845=CARTESIAN_POINT('Ctrl Pts',(74.5997654151808,27.375,74.5997654151808));
#6846=CARTESIAN_POINT('Ctrl Pts',(43.6995308303616,27.3125,105.5));
#6847=CARTESIAN_POINT('Ctrl Pts',(1.93800355965069E-14,27.25,105.5));
#6848=CARTESIAN_POINT('Ctrl Pts',(1.93800355965069E-14,28.3750000027312,
105.5));
#6849=CARTESIAN_POINT('Ctrl Pts',(-43.6995308303616,28.3125000027312,105.5));
#6850=CARTESIAN_POINT('Ctrl Pts',(-74.5997654151808,28.2500000027312,74.5997654151808));
#6851=CARTESIAN_POINT('Ctrl Pts',(-105.5,28.1875000027312,43.6995308303616));
#6852=CARTESIAN_POINT('Ctrl Pts',(-105.5,28.1250000027312,0.));
#6853=CARTESIAN_POINT('Ctrl Pts',(-105.5,28.0625000027312,-43.6995308303615));
#6854=CARTESIAN_POINT('Ctrl Pts',(-74.5997654151808,28.0000000027312,-74.5997654151808));
#6855=CARTESIAN_POINT('Ctrl Pts',(-43.6995308303615,27.9375000027312,-105.5));
#6856=CARTESIAN_POINT('Ctrl Pts',(-6.46001186550229E-15,27.8750000027312,
-105.5));
#6857=CARTESIAN_POINT('Ctrl Pts',(43.6995308303615,27.8125000027312,-105.5));
#6858=CARTESIAN_POINT('Ctrl Pts',(74.5997654151808,27.7500000027312,-74.5997654151808));
#6859=CARTESIAN_POINT('Ctrl Pts',(105.5,27.6875000027312,-43.6995308303616));
#6860=CARTESIAN_POINT('Ctrl Pts',(105.5,27.6250000027312,-1.29200237310046E-14));
#6861=CARTESIAN_POINT('Ctrl Pts',(105.5,27.5625000027312,43.6995308303615));
#6862=CARTESIAN_POINT('Ctrl Pts',(74.5997654151808,27.5000000027312,74.5997654151808));
#6863=CARTESIAN_POINT('Ctrl Pts',(43.6995308303616,27.4375000027312,105.5));
#6864=CARTESIAN_POINT('Ctrl Pts',(1.93800355965069E-14,27.3750000027312,
105.5));
#6865=CARTESIAN_POINT('Origin',(0.,105.,0.));
#6866=CARTESIAN_POINT('',(3.23000593275114E-15,29.3750000027312,105.5));
#6867=CARTESIAN_POINT('',(3.23000593275114E-15,29.25,105.5));
#6868=CARTESIAN_POINT('',(-1.29200237310046E-14,105.,105.5));
#6869=CARTESIAN_POINT('Ctrl Pts',(1.93800355965069E-14,29.25,105.5));
#6870=CARTESIAN_POINT('Ctrl Pts',(-43.6995308303616,29.1875,105.5));
#6871=CARTESIAN_POINT('Ctrl Pts',(-74.5997654151808,29.125,74.5997654151808));
#6872=CARTESIAN_POINT('Ctrl Pts',(-105.5,29.0625,43.6995308303616));
#6873=CARTESIAN_POINT('Ctrl Pts',(-105.5,29.,0.));
#6874=CARTESIAN_POINT('Ctrl Pts',(-105.5,28.9375,-43.6995308303615));
#6875=CARTESIAN_POINT('Ctrl Pts',(-74.5997654151808,28.875,-74.5997654151808));
#6876=CARTESIAN_POINT('Ctrl Pts',(-43.6995308303615,28.8125,-105.5));
#6877=CARTESIAN_POINT('Ctrl Pts',(-6.46001186550229E-15,28.75,-105.5));
#6878=CARTESIAN_POINT('Ctrl Pts',(43.6995308303615,28.6875,-105.5));
#6879=CARTESIAN_POINT('Ctrl Pts',(74.5997654151808,28.625,-74.5997654151808));
#6880=CARTESIAN_POINT('Ctrl Pts',(105.5,28.5625,-43.6995308303616));
#6881=CARTESIAN_POINT('Ctrl Pts',(105.5,28.5,-1.29200237310046E-14));
#6882=CARTESIAN_POINT('Ctrl Pts',(105.5,28.4375,43.6995308303615));
#6883=CARTESIAN_POINT('Ctrl Pts',(74.5997654151808,28.375,74.5997654151808));
#6884=CARTESIAN_POINT('Ctrl Pts',(43.6995308303616,28.3125,105.5));
#6885=CARTESIAN_POINT('Ctrl Pts',(1.93800355965069E-14,28.25,105.5));
#6886=CARTESIAN_POINT('Ctrl Pts',(1.93800355965069E-14,29.3750000027312,
105.5));
#6887=CARTESIAN_POINT('Ctrl Pts',(-43.6995308303616,29.3125000027312,105.5));
#6888=CARTESIAN_POINT('Ctrl Pts',(-74.5997654151808,29.2500000027312,74.5997654151808));
#6889=CARTESIAN_POINT('Ctrl Pts',(-105.5,29.1875000027312,43.6995308303616));
#6890=CARTESIAN_POINT('Ctrl Pts',(-105.5,29.1250000027312,0.));
#6891=CARTESIAN_POINT('Ctrl Pts',(-105.5,29.0625000027312,-43.6995308303615));
#6892=CARTESIAN_POINT('Ctrl Pts',(-74.5997654151808,29.0000000027312,-74.5997654151808));
#6893=CARTESIAN_POINT('Ctrl Pts',(-43.6995308303615,28.9375000027312,-105.5));
#6894=CARTESIAN_POINT('Ctrl Pts',(-6.46001186550229E-15,28.8750000027312,
-105.5));
#6895=CARTESIAN_POINT('Ctrl Pts',(43.6995308303615,28.8125000027312,-105.5));
#6896=CARTESIAN_POINT('Ctrl Pts',(74.5997654151808,28.7500000027312,-74.5997654151808));
#6897=CARTESIAN_POINT('Ctrl Pts',(105.5,28.6875000027312,-43.6995308303616));
#6898=CARTESIAN_POINT('Ctrl Pts',(105.5,28.6250000027312,-1.29200237310046E-14));
#6899=CARTESIAN_POINT('Ctrl Pts',(105.5,28.5625000027312,43.6995308303615));
#6900=CARTESIAN_POINT('Ctrl Pts',(74.5997654151808,28.5000000027312,74.5997654151808));
#6901=CARTESIAN_POINT('Ctrl Pts',(43.6995308303616,28.4375000027312,105.5));
#6902=CARTESIAN_POINT('Ctrl Pts',(1.93800355965069E-14,28.3750000027312,
105.5));
#6903=CARTESIAN_POINT('Origin',(0.,105.,0.));
#6904=CARTESIAN_POINT('',(3.23000593275114E-15,30.3750000027312,105.5));
#6905=CARTESIAN_POINT('',(3.23000593275114E-15,30.25,105.5));
#6906=CARTESIAN_POINT('',(-1.29200237310046E-14,105.,105.5));
#6907=CARTESIAN_POINT('Ctrl Pts',(1.93800355965069E-14,30.25,105.5));
#6908=CARTESIAN_POINT('Ctrl Pts',(-43.6995308303616,30.1875,105.5));
#6909=CARTESIAN_POINT('Ctrl Pts',(-74.5997654151808,30.125,74.5997654151808));
#6910=CARTESIAN_POINT('Ctrl Pts',(-105.5,30.0625,43.6995308303616));
#6911=CARTESIAN_POINT('Ctrl Pts',(-105.5,30.,0.));
#6912=CARTESIAN_POINT('Ctrl Pts',(-105.5,29.9375,-43.6995308303615));
#6913=CARTESIAN_POINT('Ctrl Pts',(-74.5997654151808,29.875,-74.5997654151808));
#6914=CARTESIAN_POINT('Ctrl Pts',(-43.6995308303615,29.8125,-105.5));
#6915=CARTESIAN_POINT('Ctrl Pts',(-6.46001186550229E-15,29.75,-105.5));
#6916=CARTESIAN_POINT('Ctrl Pts',(43.6995308303615,29.6875,-105.5));
#6917=CARTESIAN_POINT('Ctrl Pts',(74.5997654151808,29.625,-74.5997654151808));
#6918=CARTESIAN_POINT('Ctrl Pts',(105.5,29.5625,-43.6995308303616));
#6919=CARTESIAN_POINT('Ctrl Pts',(105.5,29.5,-1.29200237310046E-14));
#6920=CARTESIAN_POINT('Ctrl Pts',(105.5,29.4375,43.6995308303615));
#6921=CARTESIAN_POINT('Ctrl Pts',(74.5997654151808,29.375,74.5997654151808));
#6922=CARTESIAN_POINT('Ctrl Pts',(43.6995308303616,29.3125,105.5));
#6923=CARTESIAN_POINT('Ctrl Pts',(1.93800355965069E-14,29.25,105.5));
#6924=CARTESIAN_POINT('Ctrl Pts',(1.93800355965069E-14,30.3750000027312,
105.5));
#6925=CARTESIAN_POINT('Ctrl Pts',(-43.6995308303616,30.3125000027312,105.5));
#6926=CARTESIAN_POINT('Ctrl Pts',(-74.5997654151808,30.2500000027312,74.5997654151808));
#6927=CARTESIAN_POINT('Ctrl Pts',(-105.5,30.1875000027312,43.6995308303616));
#6928=CARTESIAN_POINT('Ctrl Pts',(-105.5,30.1250000027312,0.));
#6929=CARTESIAN_POINT('Ctrl Pts',(-105.5,30.0625000027312,-43.6995308303615));
#6930=CARTESIAN_POINT('Ctrl Pts',(-74.5997654151808,30.0000000027312,-74.5997654151808));
#6931=CARTESIAN_POINT('Ctrl Pts',(-43.6995308303615,29.9375000027312,-105.5));
#6932=CARTESIAN_POINT('Ctrl Pts',(-6.46001186550229E-15,29.8750000027312,
-105.5));
#6933=CARTESIAN_POINT('Ctrl Pts',(43.6995308303615,29.8125000027312,-105.5));
#6934=CARTESIAN_POINT('Ctrl Pts',(74.5997654151808,29.7500000027312,-74.5997654151808));
#6935=CARTESIAN_POINT('Ctrl Pts',(105.5,29.6875000027312,-43.6995308303616));
#6936=CARTESIAN_POINT('Ctrl Pts',(105.5,29.6250000027312,-1.29200237310046E-14));
#6937=CARTESIAN_POINT('Ctrl Pts',(105.5,29.5625000027312,43.6995308303615));
#6938=CARTESIAN_POINT('Ctrl Pts',(74.5997654151808,29.5000000027312,74.5997654151808));
#6939=CARTESIAN_POINT('Ctrl Pts',(43.6995308303616,29.4375000027312,105.5));
#6940=CARTESIAN_POINT('Ctrl Pts',(1.93800355965069E-14,29.3750000027312,
105.5));
#6941=CARTESIAN_POINT('Origin',(0.,105.,0.));
#6942=CARTESIAN_POINT('',(3.23000593275114E-15,31.3750000027312,105.5));
#6943=CARTESIAN_POINT('',(3.23000593275114E-15,31.25,105.5));
#6944=CARTESIAN_POINT('',(-1.29200237310046E-14,105.,105.5));
#6945=CARTESIAN_POINT('Ctrl Pts',(1.93800355965069E-14,31.25,105.5));
#6946=CARTESIAN_POINT('Ctrl Pts',(-43.6995308303616,31.1875,105.5));
#6947=CARTESIAN_POINT('Ctrl Pts',(-74.5997654151808,31.125,74.5997654151808));
#6948=CARTESIAN_POINT('Ctrl Pts',(-105.5,31.0625,43.6995308303616));
#6949=CARTESIAN_POINT('Ctrl Pts',(-105.5,31.,0.));
#6950=CARTESIAN_POINT('Ctrl Pts',(-105.5,30.9375,-43.6995308303615));
#6951=CARTESIAN_POINT('Ctrl Pts',(-74.5997654151808,30.875,-74.5997654151808));
#6952=CARTESIAN_POINT('Ctrl Pts',(-43.6995308303615,30.8125,-105.5));
#6953=CARTESIAN_POINT('Ctrl Pts',(-6.46001186550229E-15,30.75,-105.5));
#6954=CARTESIAN_POINT('Ctrl Pts',(43.6995308303615,30.6875,-105.5));
#6955=CARTESIAN_POINT('Ctrl Pts',(74.5997654151808,30.625,-74.5997654151808));
#6956=CARTESIAN_POINT('Ctrl Pts',(105.5,30.5625,-43.6995308303616));
#6957=CARTESIAN_POINT('Ctrl Pts',(105.5,30.5,-1.29200237310046E-14));
#6958=CARTESIAN_POINT('Ctrl Pts',(105.5,30.4375,43.6995308303615));
#6959=CARTESIAN_POINT('Ctrl Pts',(74.5997654151808,30.375,74.5997654151808));
#6960=CARTESIAN_POINT('Ctrl Pts',(43.6995308303616,30.3125,105.5));
#6961=CARTESIAN_POINT('Ctrl Pts',(1.93800355965069E-14,30.25,105.5));
#6962=CARTESIAN_POINT('Ctrl Pts',(1.93800355965069E-14,31.3750000027312,
105.5));
#6963=CARTESIAN_POINT('Ctrl Pts',(-43.6995308303616,31.3125000027312,105.5));
#6964=CARTESIAN_POINT('Ctrl Pts',(-74.5997654151808,31.2500000027312,74.5997654151808));
#6965=CARTESIAN_POINT('Ctrl Pts',(-105.5,31.1875000027312,43.6995308303616));
#6966=CARTESIAN_POINT('Ctrl Pts',(-105.5,31.1250000027312,0.));
#6967=CARTESIAN_POINT('Ctrl Pts',(-105.5,31.0625000027312,-43.6995308303615));
#6968=CARTESIAN_POINT('Ctrl Pts',(-74.5997654151808,31.0000000027312,-74.5997654151808));
#6969=CARTESIAN_POINT('Ctrl Pts',(-43.6995308303615,30.9375000027312,-105.5));
#6970=CARTESIAN_POINT('Ctrl Pts',(-6.46001186550229E-15,30.8750000027312,
-105.5));
#6971=CARTESIAN_POINT('Ctrl Pts',(43.6995308303615,30.8125000027312,-105.5));
#6972=CARTESIAN_POINT('Ctrl Pts',(74.5997654151808,30.7500000027312,-74.5997654151808));
#6973=CARTESIAN_POINT('Ctrl Pts',(105.5,30.6875000027312,-43.6995308303616));
#6974=CARTESIAN_POINT('Ctrl Pts',(105.5,30.6250000027312,-1.29200237310046E-14));
#6975=CARTESIAN_POINT('Ctrl Pts',(105.5,30.5625000027312,43.6995308303615));
#6976=CARTESIAN_POINT('Ctrl Pts',(74.5997654151808,30.5000000027312,74.5997654151808));
#6977=CARTESIAN_POINT('Ctrl Pts',(43.6995308303616,30.4375000027312,105.5));
#6978=CARTESIAN_POINT('Ctrl Pts',(1.93800355965069E-14,30.3750000027312,
105.5));
#6979=CARTESIAN_POINT('Origin',(0.,105.,0.));
#6980=CARTESIAN_POINT('',(3.23000593275114E-15,32.3750000027312,105.5));
#6981=CARTESIAN_POINT('',(3.23000593275114E-15,32.25,105.5));
#6982=CARTESIAN_POINT('',(-1.29200237310046E-14,105.,105.5));
#6983=CARTESIAN_POINT('Ctrl Pts',(1.93800355965069E-14,32.25,105.5));
#6984=CARTESIAN_POINT('Ctrl Pts',(-43.6995308303616,32.1875,105.5));
#6985=CARTESIAN_POINT('Ctrl Pts',(-74.5997654151808,32.125,74.5997654151808));
#6986=CARTESIAN_POINT('Ctrl Pts',(-105.5,32.0625,43.6995308303616));
#6987=CARTESIAN_POINT('Ctrl Pts',(-105.5,32.,0.));
#6988=CARTESIAN_POINT('Ctrl Pts',(-105.5,31.9375,-43.6995308303615));
#6989=CARTESIAN_POINT('Ctrl Pts',(-74.5997654151808,31.875,-74.5997654151808));
#6990=CARTESIAN_POINT('Ctrl Pts',(-43.6995308303615,31.8125,-105.5));
#6991=CARTESIAN_POINT('Ctrl Pts',(-6.46001186550229E-15,31.75,-105.5));
#6992=CARTESIAN_POINT('Ctrl Pts',(43.6995308303615,31.6875,-105.5));
#6993=CARTESIAN_POINT('Ctrl Pts',(74.5997654151808,31.625,-74.5997654151808));
#6994=CARTESIAN_POINT('Ctrl Pts',(105.5,31.5625,-43.6995308303616));
#6995=CARTESIAN_POINT('Ctrl Pts',(105.5,31.5,-1.29200237310046E-14));
#6996=CARTESIAN_POINT('Ctrl Pts',(105.5,31.4375,43.6995308303615));
#6997=CARTESIAN_POINT('Ctrl Pts',(74.5997654151808,31.375,74.5997654151808));
#6998=CARTESIAN_POINT('Ctrl Pts',(43.6995308303616,31.3125,105.5));
#6999=CARTESIAN_POINT('Ctrl Pts',(1.93800355965069E-14,31.25,105.5));
#7000=CARTESIAN_POINT('Ctrl Pts',(1.93800355965069E-14,32.3750000027312,
105.5));
#7001=CARTESIAN_POINT('Ctrl Pts',(-43.6995308303616,32.3125000027312,105.5));
#7002=CARTESIAN_POINT('Ctrl Pts',(-74.5997654151808,32.2500000027312,74.5997654151808));
#7003=CARTESIAN_POINT('Ctrl Pts',(-105.5,32.1875000027312,43.6995308303616));
#7004=CARTESIAN_POINT('Ctrl Pts',(-105.5,32.1250000027312,0.));
#7005=CARTESIAN_POINT('Ctrl Pts',(-105.5,32.0625000027312,-43.6995308303615));
#7006=CARTESIAN_POINT('Ctrl Pts',(-74.5997654151808,32.0000000027312,-74.5997654151808));
#7007=CARTESIAN_POINT('Ctrl Pts',(-43.6995308303615,31.9375000027312,-105.5));
#7008=CARTESIAN_POINT('Ctrl Pts',(-6.46001186550229E-15,31.8750000027312,
-105.5));
#7009=CARTESIAN_POINT('Ctrl Pts',(43.6995308303615,31.8125000027312,-105.5));
#7010=CARTESIAN_POINT('Ctrl Pts',(74.5997654151808,31.7500000027312,-74.5997654151808));
#7011=CARTESIAN_POINT('Ctrl Pts',(105.5,31.6875000027312,-43.6995308303616));
#7012=CARTESIAN_POINT('Ctrl Pts',(105.5,31.6250000027312,-1.29200237310046E-14));
#7013=CARTESIAN_POINT('Ctrl Pts',(105.5,31.5625000027312,43.6995308303615));
#7014=CARTESIAN_POINT('Ctrl Pts',(74.5997654151808,31.5000000027312,74.5997654151808));
#7015=CARTESIAN_POINT('Ctrl Pts',(43.6995308303616,31.4375000027312,105.5));
#7016=CARTESIAN_POINT('Ctrl Pts',(1.93800355965069E-14,31.3750000027312,
105.5));
#7017=CARTESIAN_POINT('Origin',(0.,105.,0.));
#7018=CARTESIAN_POINT('',(3.23000593275114E-15,33.3750000027312,105.5));
#7019=CARTESIAN_POINT('',(3.23000593275114E-15,33.25,105.5));
#7020=CARTESIAN_POINT('',(-1.29200237310046E-14,105.,105.5));
#7021=CARTESIAN_POINT('Ctrl Pts',(1.93800355965069E-14,33.25,105.5));
#7022=CARTESIAN_POINT('Ctrl Pts',(-43.6995308303616,33.1875,105.5));
#7023=CARTESIAN_POINT('Ctrl Pts',(-74.5997654151808,33.125,74.5997654151808));
#7024=CARTESIAN_POINT('Ctrl Pts',(-105.5,33.0625,43.6995308303616));
#7025=CARTESIAN_POINT('Ctrl Pts',(-105.5,33.,0.));
#7026=CARTESIAN_POINT('Ctrl Pts',(-105.5,32.9375,-43.6995308303615));
#7027=CARTESIAN_POINT('Ctrl Pts',(-74.5997654151808,32.875,-74.5997654151808));
#7028=CARTESIAN_POINT('Ctrl Pts',(-43.6995308303615,32.8125,-105.5));
#7029=CARTESIAN_POINT('Ctrl Pts',(-6.46001186550229E-15,32.75,-105.5));
#7030=CARTESIAN_POINT('Ctrl Pts',(43.6995308303615,32.6875,-105.5));
#7031=CARTESIAN_POINT('Ctrl Pts',(74.5997654151808,32.625,-74.5997654151808));
#7032=CARTESIAN_POINT('Ctrl Pts',(105.5,32.5625,-43.6995308303616));
#7033=CARTESIAN_POINT('Ctrl Pts',(105.5,32.5,-1.29200237310046E-14));
#7034=CARTESIAN_POINT('Ctrl Pts',(105.5,32.4375,43.6995308303615));
#7035=CARTESIAN_POINT('Ctrl Pts',(74.5997654151808,32.375,74.5997654151808));
#7036=CARTESIAN_POINT('Ctrl Pts',(43.6995308303616,32.3125,105.5));
#7037=CARTESIAN_POINT('Ctrl Pts',(1.93800355965069E-14,32.25,105.5));
#7038=CARTESIAN_POINT('Ctrl Pts',(1.93800355965069E-14,33.3750000027312,
105.5));
#7039=CARTESIAN_POINT('Ctrl Pts',(-43.6995308303616,33.3125000027312,105.5));
#7040=CARTESIAN_POINT('Ctrl Pts',(-74.5997654151808,33.2500000027312,74.5997654151808));
#7041=CARTESIAN_POINT('Ctrl Pts',(-105.5,33.1875000027312,43.6995308303616));
#7042=CARTESIAN_POINT('Ctrl Pts',(-105.5,33.1250000027312,0.));
#7043=CARTESIAN_POINT('Ctrl Pts',(-105.5,33.0625000027312,-43.6995308303615));
#7044=CARTESIAN_POINT('Ctrl Pts',(-74.5997654151808,33.0000000027312,-74.5997654151808));
#7045=CARTESIAN_POINT('Ctrl Pts',(-43.6995308303615,32.9375000027312,-105.5));
#7046=CARTESIAN_POINT('Ctrl Pts',(-6.46001186550229E-15,32.8750000027312,
-105.5));
#7047=CARTESIAN_POINT('Ctrl Pts',(43.6995308303615,32.8125000027312,-105.5));
#7048=CARTESIAN_POINT('Ctrl Pts',(74.5997654151808,32.7500000027312,-74.5997654151808));
#7049=CARTESIAN_POINT('Ctrl Pts',(105.5,32.6875000027312,-43.6995308303616));
#7050=CARTESIAN_POINT('Ctrl Pts',(105.5,32.6250000027312,-1.29200237310046E-14));
#7051=CARTESIAN_POINT('Ctrl Pts',(105.5,32.5625000027312,43.6995308303615));
#7052=CARTESIAN_POINT('Ctrl Pts',(74.5997654151808,32.5000000027312,74.5997654151808));
#7053=CARTESIAN_POINT('Ctrl Pts',(43.6995308303616,32.4375000027312,105.5));
#7054=CARTESIAN_POINT('Ctrl Pts',(1.93800355965069E-14,32.3750000027312,
105.5));
#7055=CARTESIAN_POINT('Origin',(0.,105.,0.));
#7056=CARTESIAN_POINT('',(3.23000593275114E-15,34.3750000027312,105.5));
#7057=CARTESIAN_POINT('',(3.23000593275114E-15,34.25,105.5));
#7058=CARTESIAN_POINT('',(-1.29200237310046E-14,105.,105.5));
#7059=CARTESIAN_POINT('Ctrl Pts',(1.93800355965069E-14,34.25,105.5));
#7060=CARTESIAN_POINT('Ctrl Pts',(-43.6995308303616,34.1875,105.5));
#7061=CARTESIAN_POINT('Ctrl Pts',(-74.5997654151808,34.125,74.5997654151808));
#7062=CARTESIAN_POINT('Ctrl Pts',(-105.5,34.0625,43.6995308303616));
#7063=CARTESIAN_POINT('Ctrl Pts',(-105.5,34.,0.));
#7064=CARTESIAN_POINT('Ctrl Pts',(-105.5,33.9375,-43.6995308303615));
#7065=CARTESIAN_POINT('Ctrl Pts',(-74.5997654151808,33.875,-74.5997654151808));
#7066=CARTESIAN_POINT('Ctrl Pts',(-43.6995308303615,33.8125,-105.5));
#7067=CARTESIAN_POINT('Ctrl Pts',(-6.46001186550229E-15,33.75,-105.5));
#7068=CARTESIAN_POINT('Ctrl Pts',(43.6995308303615,33.6875,-105.5));
#7069=CARTESIAN_POINT('Ctrl Pts',(74.5997654151808,33.625,-74.5997654151808));
#7070=CARTESIAN_POINT('Ctrl Pts',(105.5,33.5625,-43.6995308303616));
#7071=CARTESIAN_POINT('Ctrl Pts',(105.5,33.5,-1.29200237310046E-14));
#7072=CARTESIAN_POINT('Ctrl Pts',(105.5,33.4375,43.6995308303615));
#7073=CARTESIAN_POINT('Ctrl Pts',(74.5997654151808,33.375,74.5997654151808));
#7074=CARTESIAN_POINT('Ctrl Pts',(43.6995308303616,33.3125,105.5));
#7075=CARTESIAN_POINT('Ctrl Pts',(1.93800355965069E-14,33.25,105.5));
#7076=CARTESIAN_POINT('Ctrl Pts',(1.93800355965069E-14,34.3750000027312,
105.5));
#7077=CARTESIAN_POINT('Ctrl Pts',(-43.6995308303616,34.3125000027312,105.5));
#7078=CARTESIAN_POINT('Ctrl Pts',(-74.5997654151808,34.2500000027312,74.5997654151808));
#7079=CARTESIAN_POINT('Ctrl Pts',(-105.5,34.1875000027312,43.6995308303616));
#7080=CARTESIAN_POINT('Ctrl Pts',(-105.5,34.1250000027312,0.));
#7081=CARTESIAN_POINT('Ctrl Pts',(-105.5,34.0625000027312,-43.6995308303615));
#7082=CARTESIAN_POINT('Ctrl Pts',(-74.5997654151808,34.0000000027312,-74.5997654151808));
#7083=CARTESIAN_POINT('Ctrl Pts',(-43.6995308303615,33.9375000027312,-105.5));
#7084=CARTESIAN_POINT('Ctrl Pts',(-6.46001186550229E-15,33.8750000027312,
-105.5));
#7085=CARTESIAN_POINT('Ctrl Pts',(43.6995308303615,33.8125000027312,-105.5));
#7086=CARTESIAN_POINT('Ctrl Pts',(74.5997654151808,33.7500000027312,-74.5997654151808));
#7087=CARTESIAN_POINT('Ctrl Pts',(105.5,33.6875000027312,-43.6995308303616));
#7088=CARTESIAN_POINT('Ctrl Pts',(105.5,33.6250000027312,-1.29200237310046E-14));
#7089=CARTESIAN_POINT('Ctrl Pts',(105.5,33.5625000027312,43.6995308303615));
#7090=CARTESIAN_POINT('Ctrl Pts',(74.5997654151808,33.5000000027312,74.5997654151808));
#7091=CARTESIAN_POINT('Ctrl Pts',(43.6995308303616,33.4375000027312,105.5));
#7092=CARTESIAN_POINT('Ctrl Pts',(1.93800355965069E-14,33.3750000027312,
105.5));
#7093=CARTESIAN_POINT('Origin',(0.,105.,0.));
#7094=CARTESIAN_POINT('',(3.23000593275114E-15,35.3750000027312,105.5));
#7095=CARTESIAN_POINT('',(3.23000593275114E-15,35.25,105.5));
#7096=CARTESIAN_POINT('',(-1.29200237310046E-14,105.,105.5));
#7097=CARTESIAN_POINT('Ctrl Pts',(1.93800355965069E-14,35.25,105.5));
#7098=CARTESIAN_POINT('Ctrl Pts',(-43.6995308303616,35.1875,105.5));
#7099=CARTESIAN_POINT('Ctrl Pts',(-74.5997654151808,35.125,74.5997654151808));
#7100=CARTESIAN_POINT('Ctrl Pts',(-105.5,35.0625,43.6995308303616));
#7101=CARTESIAN_POINT('Ctrl Pts',(-105.5,35.,0.));
#7102=CARTESIAN_POINT('Ctrl Pts',(-105.5,34.9375,-43.6995308303615));
#7103=CARTESIAN_POINT('Ctrl Pts',(-74.5997654151808,34.875,-74.5997654151808));
#7104=CARTESIAN_POINT('Ctrl Pts',(-43.6995308303615,34.8125,-105.5));
#7105=CARTESIAN_POINT('Ctrl Pts',(-6.46001186550229E-15,34.75,-105.5));
#7106=CARTESIAN_POINT('Ctrl Pts',(43.6995308303615,34.6875,-105.5));
#7107=CARTESIAN_POINT('Ctrl Pts',(74.5997654151808,34.625,-74.5997654151808));
#7108=CARTESIAN_POINT('Ctrl Pts',(105.5,34.5625,-43.6995308303616));
#7109=CARTESIAN_POINT('Ctrl Pts',(105.5,34.5,-1.29200237310046E-14));
#7110=CARTESIAN_POINT('Ctrl Pts',(105.5,34.4375,43.6995308303615));
#7111=CARTESIAN_POINT('Ctrl Pts',(74.5997654151808,34.375,74.5997654151808));
#7112=CARTESIAN_POINT('Ctrl Pts',(43.6995308303616,34.3125,105.5));
#7113=CARTESIAN_POINT('Ctrl Pts',(1.93800355965069E-14,34.25,105.5));
#7114=CARTESIAN_POINT('Ctrl Pts',(1.93800355965069E-14,35.3750000027312,
105.5));
#7115=CARTESIAN_POINT('Ctrl Pts',(-43.6995308303616,35.3125000027312,105.5));
#7116=CARTESIAN_POINT('Ctrl Pts',(-74.5997654151808,35.2500000027312,74.5997654151808));
#7117=CARTESIAN_POINT('Ctrl Pts',(-105.5,35.1875000027312,43.6995308303616));
#7118=CARTESIAN_POINT('Ctrl Pts',(-105.5,35.1250000027312,0.));
#7119=CARTESIAN_POINT('Ctrl Pts',(-105.5,35.0625000027312,-43.6995308303615));
#7120=CARTESIAN_POINT('Ctrl Pts',(-74.5997654151808,35.0000000027312,-74.5997654151808));
#7121=CARTESIAN_POINT('Ctrl Pts',(-43.6995308303615,34.9375000027312,-105.5));
#7122=CARTESIAN_POINT('Ctrl Pts',(-6.46001186550229E-15,34.8750000027312,
-105.5));
#7123=CARTESIAN_POINT('Ctrl Pts',(43.6995308303615,34.8125000027312,-105.5));
#7124=CARTESIAN_POINT('Ctrl Pts',(74.5997654151808,34.7500000027312,-74.5997654151808));
#7125=CARTESIAN_POINT('Ctrl Pts',(105.5,34.6875000027312,-43.6995308303616));
#7126=CARTESIAN_POINT('Ctrl Pts',(105.5,34.6250000027312,-1.29200237310046E-14));
#7127=CARTESIAN_POINT('Ctrl Pts',(105.5,34.5625000027312,43.6995308303615));
#7128=CARTESIAN_POINT('Ctrl Pts',(74.5997654151808,34.5000000027312,74.5997654151808));
#7129=CARTESIAN_POINT('Ctrl Pts',(43.6995308303616,34.4375000027312,105.5));
#7130=CARTESIAN_POINT('Ctrl Pts',(1.93800355965069E-14,34.3750000027312,
105.5));
#7131=CARTESIAN_POINT('Origin',(0.,105.,0.));
#7132=CARTESIAN_POINT('',(3.23000593275114E-15,36.3750000027312,105.5));
#7133=CARTESIAN_POINT('',(3.23000593275114E-15,36.25,105.5));
#7134=CARTESIAN_POINT('',(-1.29200237310046E-14,105.,105.5));
#7135=CARTESIAN_POINT('Ctrl Pts',(1.93800355965069E-14,36.25,105.5));
#7136=CARTESIAN_POINT('Ctrl Pts',(-43.6995308303616,36.1875,105.5));
#7137=CARTESIAN_POINT('Ctrl Pts',(-74.5997654151808,36.125,74.5997654151808));
#7138=CARTESIAN_POINT('Ctrl Pts',(-105.5,36.0625,43.6995308303616));
#7139=CARTESIAN_POINT('Ctrl Pts',(-105.5,36.,0.));
#7140=CARTESIAN_POINT('Ctrl Pts',(-105.5,35.9375,-43.6995308303615));
#7141=CARTESIAN_POINT('Ctrl Pts',(-74.5997654151808,35.875,-74.5997654151808));
#7142=CARTESIAN_POINT('Ctrl Pts',(-43.6995308303615,35.8125,-105.5));
#7143=CARTESIAN_POINT('Ctrl Pts',(-6.46001186550229E-15,35.75,-105.5));
#7144=CARTESIAN_POINT('Ctrl Pts',(43.6995308303615,35.6875,-105.5));
#7145=CARTESIAN_POINT('Ctrl Pts',(74.5997654151808,35.625,-74.5997654151808));
#7146=CARTESIAN_POINT('Ctrl Pts',(105.5,35.5625,-43.6995308303616));
#7147=CARTESIAN_POINT('Ctrl Pts',(105.5,35.5,-1.29200237310046E-14));
#7148=CARTESIAN_POINT('Ctrl Pts',(105.5,35.4375,43.6995308303615));
#7149=CARTESIAN_POINT('Ctrl Pts',(74.5997654151808,35.375,74.5997654151808));
#7150=CARTESIAN_POINT('Ctrl Pts',(43.6995308303616,35.3125,105.5));
#7151=CARTESIAN_POINT('Ctrl Pts',(1.93800355965069E-14,35.25,105.5));
#7152=CARTESIAN_POINT('Ctrl Pts',(1.93800355965069E-14,36.3750000027312,
105.5));
#7153=CARTESIAN_POINT('Ctrl Pts',(-43.6995308303616,36.3125000027312,105.5));
#7154=CARTESIAN_POINT('Ctrl Pts',(-74.5997654151808,36.2500000027312,74.5997654151808));
#7155=CARTESIAN_POINT('Ctrl Pts',(-105.5,36.1875000027312,43.6995308303616));
#7156=CARTESIAN_POINT('Ctrl Pts',(-105.5,36.1250000027312,0.));
#7157=CARTESIAN_POINT('Ctrl Pts',(-105.5,36.0625000027312,-43.6995308303615));
#7158=CARTESIAN_POINT('Ctrl Pts',(-74.5997654151808,36.0000000027312,-74.5997654151808));
#7159=CARTESIAN_POINT('Ctrl Pts',(-43.6995308303615,35.9375000027312,-105.5));
#7160=CARTESIAN_POINT('Ctrl Pts',(-6.46001186550229E-15,35.8750000027312,
-105.5));
#7161=CARTESIAN_POINT('Ctrl Pts',(43.6995308303615,35.8125000027312,-105.5));
#7162=CARTESIAN_POINT('Ctrl Pts',(74.5997654151808,35.7500000027312,-74.5997654151808));
#7163=CARTESIAN_POINT('Ctrl Pts',(105.5,35.6875000027312,-43.6995308303616));
#7164=CARTESIAN_POINT('Ctrl Pts',(105.5,35.6250000027312,-1.29200237310046E-14));
#7165=CARTESIAN_POINT('Ctrl Pts',(105.5,35.5625000027312,43.6995308303615));
#7166=CARTESIAN_POINT('Ctrl Pts',(74.5997654151808,35.5000000027312,74.5997654151808));
#7167=CARTESIAN_POINT('Ctrl Pts',(43.6995308303616,35.4375000027312,105.5));
#7168=CARTESIAN_POINT('Ctrl Pts',(1.93800355965069E-14,35.3750000027312,
105.5));
#7169=CARTESIAN_POINT('Origin',(0.,105.,0.));
#7170=CARTESIAN_POINT('',(3.23000593275114E-15,37.3750000027312,105.5));
#7171=CARTESIAN_POINT('',(3.23000593275114E-15,37.25,105.5));
#7172=CARTESIAN_POINT('',(-1.29200237310046E-14,105.,105.5));
#7173=CARTESIAN_POINT('Ctrl Pts',(1.93800355965069E-14,37.25,105.5));
#7174=CARTESIAN_POINT('Ctrl Pts',(-43.6995308303616,37.1875,105.5));
#7175=CARTESIAN_POINT('Ctrl Pts',(-74.5997654151808,37.125,74.5997654151808));
#7176=CARTESIAN_POINT('Ctrl Pts',(-105.5,37.0625,43.6995308303616));
#7177=CARTESIAN_POINT('Ctrl Pts',(-105.5,37.,0.));
#7178=CARTESIAN_POINT('Ctrl Pts',(-105.5,36.9375,-43.6995308303615));
#7179=CARTESIAN_POINT('Ctrl Pts',(-74.5997654151808,36.875,-74.5997654151808));
#7180=CARTESIAN_POINT('Ctrl Pts',(-43.6995308303615,36.8125,-105.5));
#7181=CARTESIAN_POINT('Ctrl Pts',(-6.46001186550229E-15,36.75,-105.5));
#7182=CARTESIAN_POINT('Ctrl Pts',(43.6995308303615,36.6875,-105.5));
#7183=CARTESIAN_POINT('Ctrl Pts',(74.5997654151808,36.625,-74.5997654151808));
#7184=CARTESIAN_POINT('Ctrl Pts',(105.5,36.5625,-43.6995308303616));
#7185=CARTESIAN_POINT('Ctrl Pts',(105.5,36.5,-1.29200237310046E-14));
#7186=CARTESIAN_POINT('Ctrl Pts',(105.5,36.4375,43.6995308303615));
#7187=CARTESIAN_POINT('Ctrl Pts',(74.5997654151808,36.375,74.5997654151808));
#7188=CARTESIAN_POINT('Ctrl Pts',(43.6995308303616,36.3125,105.5));
#7189=CARTESIAN_POINT('Ctrl Pts',(1.93800355965069E-14,36.25,105.5));
#7190=CARTESIAN_POINT('Ctrl Pts',(1.93800355965069E-14,37.3750000027312,
105.5));
#7191=CARTESIAN_POINT('Ctrl Pts',(-43.6995308303616,37.3125000027312,105.5));
#7192=CARTESIAN_POINT('Ctrl Pts',(-74.5997654151808,37.2500000027312,74.5997654151808));
#7193=CARTESIAN_POINT('Ctrl Pts',(-105.5,37.1875000027312,43.6995308303616));
#7194=CARTESIAN_POINT('Ctrl Pts',(-105.5,37.1250000027312,0.));
#7195=CARTESIAN_POINT('Ctrl Pts',(-105.5,37.0625000027312,-43.6995308303615));
#7196=CARTESIAN_POINT('Ctrl Pts',(-74.5997654151808,37.0000000027312,-74.5997654151808));
#7197=CARTESIAN_POINT('Ctrl Pts',(-43.6995308303615,36.9375000027312,-105.5));
#7198=CARTESIAN_POINT('Ctrl Pts',(-6.46001186550229E-15,36.8750000027312,
-105.5));
#7199=CARTESIAN_POINT('Ctrl Pts',(43.6995308303615,36.8125000027312,-105.5));
#7200=CARTESIAN_POINT('Ctrl Pts',(74.5997654151808,36.7500000027312,-74.5997654151808));
#7201=CARTESIAN_POINT('Ctrl Pts',(105.5,36.6875000027312,-43.6995308303616));
#7202=CARTESIAN_POINT('Ctrl Pts',(105.5,36.6250000027312,-1.29200237310046E-14));
#7203=CARTESIAN_POINT('Ctrl Pts',(105.5,36.5625000027312,43.6995308303615));
#7204=CARTESIAN_POINT('Ctrl Pts',(74.5997654151808,36.5000000027312,74.5997654151808));
#7205=CARTESIAN_POINT('Ctrl Pts',(43.6995308303616,36.4375000027312,105.5));
#7206=CARTESIAN_POINT('Ctrl Pts',(1.93800355965069E-14,36.3750000027312,
105.5));
#7207=CARTESIAN_POINT('Origin',(0.,105.,0.));
#7208=CARTESIAN_POINT('',(3.23000593275114E-15,38.3750000027312,105.5));
#7209=CARTESIAN_POINT('',(3.23000593275114E-15,38.25,105.5));
#7210=CARTESIAN_POINT('',(-1.29200237310046E-14,105.,105.5));
#7211=CARTESIAN_POINT('Ctrl Pts',(1.93800355965069E-14,38.25,105.5));
#7212=CARTESIAN_POINT('Ctrl Pts',(-43.6995308303616,38.1875,105.5));
#7213=CARTESIAN_POINT('Ctrl Pts',(-74.5997654151808,38.125,74.5997654151808));
#7214=CARTESIAN_POINT('Ctrl Pts',(-105.5,38.0625,43.6995308303616));
#7215=CARTESIAN_POINT('Ctrl Pts',(-105.5,38.,0.));
#7216=CARTESIAN_POINT('Ctrl Pts',(-105.5,37.9375,-43.6995308303615));
#7217=CARTESIAN_POINT('Ctrl Pts',(-74.5997654151808,37.875,-74.5997654151808));
#7218=CARTESIAN_POINT('Ctrl Pts',(-43.6995308303615,37.8125,-105.5));
#7219=CARTESIAN_POINT('Ctrl Pts',(-6.46001186550229E-15,37.75,-105.5));
#7220=CARTESIAN_POINT('Ctrl Pts',(43.6995308303615,37.6875,-105.5));
#7221=CARTESIAN_POINT('Ctrl Pts',(74.5997654151808,37.625,-74.5997654151808));
#7222=CARTESIAN_POINT('Ctrl Pts',(105.5,37.5625,-43.6995308303616));
#7223=CARTESIAN_POINT('Ctrl Pts',(105.5,37.5,-1.29200237310046E-14));
#7224=CARTESIAN_POINT('Ctrl Pts',(105.5,37.4375,43.6995308303615));
#7225=CARTESIAN_POINT('Ctrl Pts',(74.5997654151808,37.375,74.5997654151808));
#7226=CARTESIAN_POINT('Ctrl Pts',(43.6995308303616,37.3125,105.5));
#7227=CARTESIAN_POINT('Ctrl Pts',(1.93800355965069E-14,37.25,105.5));
#7228=CARTESIAN_POINT('Ctrl Pts',(1.93800355965069E-14,38.3750000027312,
105.5));
#7229=CARTESIAN_POINT('Ctrl Pts',(-43.6995308303616,38.3125000027312,105.5));
#7230=CARTESIAN_POINT('Ctrl Pts',(-74.5997654151808,38.2500000027312,74.5997654151808));
#7231=CARTESIAN_POINT('Ctrl Pts',(-105.5,38.1875000027312,43.6995308303616));
#7232=CARTESIAN_POINT('Ctrl Pts',(-105.5,38.1250000027312,0.));
#7233=CARTESIAN_POINT('Ctrl Pts',(-105.5,38.0625000027312,-43.6995308303615));
#7234=CARTESIAN_POINT('Ctrl Pts',(-74.5997654151808,38.0000000027312,-74.5997654151808));
#7235=CARTESIAN_POINT('Ctrl Pts',(-43.6995308303615,37.9375000027312,-105.5));
#7236=CARTESIAN_POINT('Ctrl Pts',(-6.46001186550229E-15,37.8750000027312,
-105.5));
#7237=CARTESIAN_POINT('Ctrl Pts',(43.6995308303615,37.8125000027312,-105.5));
#7238=CARTESIAN_POINT('Ctrl Pts',(74.5997654151808,37.7500000027312,-74.5997654151808));
#7239=CARTESIAN_POINT('Ctrl Pts',(105.5,37.6875000027312,-43.6995308303616));
#7240=CARTESIAN_POINT('Ctrl Pts',(105.5,37.6250000027312,-1.29200237310046E-14));
#7241=CARTESIAN_POINT('Ctrl Pts',(105.5,37.5625000027312,43.6995308303615));
#7242=CARTESIAN_POINT('Ctrl Pts',(74.5997654151808,37.5000000027312,74.5997654151808));
#7243=CARTESIAN_POINT('Ctrl Pts',(43.6995308303616,37.4375000027312,105.5));
#7244=CARTESIAN_POINT('Ctrl Pts',(1.93800355965069E-14,37.3750000027312,
105.5));
#7245=CARTESIAN_POINT('Origin',(0.,105.,0.));
#7246=CARTESIAN_POINT('',(3.23000593275114E-15,39.3750000027312,105.5));
#7247=CARTESIAN_POINT('',(3.23000593275114E-15,39.25,105.5));
#7248=CARTESIAN_POINT('',(-1.29200237310046E-14,105.,105.5));
#7249=CARTESIAN_POINT('Ctrl Pts',(1.93800355965069E-14,39.25,105.5));
#7250=CARTESIAN_POINT('Ctrl Pts',(-43.6995308303616,39.1875,105.5));
#7251=CARTESIAN_POINT('Ctrl Pts',(-74.5997654151808,39.125,74.5997654151808));
#7252=CARTESIAN_POINT('Ctrl Pts',(-105.5,39.0625,43.6995308303616));
#7253=CARTESIAN_POINT('Ctrl Pts',(-105.5,39.,0.));
#7254=CARTESIAN_POINT('Ctrl Pts',(-105.5,38.9375,-43.6995308303615));
#7255=CARTESIAN_POINT('Ctrl Pts',(-74.5997654151808,38.875,-74.5997654151808));
#7256=CARTESIAN_POINT('Ctrl Pts',(-43.6995308303615,38.8125,-105.5));
#7257=CARTESIAN_POINT('Ctrl Pts',(-6.46001186550229E-15,38.75,-105.5));
#7258=CARTESIAN_POINT('Ctrl Pts',(43.6995308303615,38.6875,-105.5));
#7259=CARTESIAN_POINT('Ctrl Pts',(74.5997654151808,38.625,-74.5997654151808));
#7260=CARTESIAN_POINT('Ctrl Pts',(105.5,38.5625,-43.6995308303616));
#7261=CARTESIAN_POINT('Ctrl Pts',(105.5,38.5,-1.29200237310046E-14));
#7262=CARTESIAN_POINT('Ctrl Pts',(105.5,38.4375,43.6995308303615));
#7263=CARTESIAN_POINT('Ctrl Pts',(74.5997654151808,38.375,74.5997654151808));
#7264=CARTESIAN_POINT('Ctrl Pts',(43.6995308303616,38.3125,105.5));
#7265=CARTESIAN_POINT('Ctrl Pts',(1.93800355965069E-14,38.25,105.5));
#7266=CARTESIAN_POINT('Ctrl Pts',(1.93800355965069E-14,39.3750000027312,
105.5));
#7267=CARTESIAN_POINT('Ctrl Pts',(-43.6995308303616,39.3125000027312,105.5));
#7268=CARTESIAN_POINT('Ctrl Pts',(-74.5997654151808,39.2500000027312,74.5997654151808));
#7269=CARTESIAN_POINT('Ctrl Pts',(-105.5,39.1875000027312,43.6995308303616));
#7270=CARTESIAN_POINT('Ctrl Pts',(-105.5,39.1250000027312,0.));
#7271=CARTESIAN_POINT('Ctrl Pts',(-105.5,39.0625000027312,-43.6995308303615));
#7272=CARTESIAN_POINT('Ctrl Pts',(-74.5997654151808,39.0000000027312,-74.5997654151808));
#7273=CARTESIAN_POINT('Ctrl Pts',(-43.6995308303615,38.9375000027312,-105.5));
#7274=CARTESIAN_POINT('Ctrl Pts',(-6.46001186550229E-15,38.8750000027312,
-105.5));
#7275=CARTESIAN_POINT('Ctrl Pts',(43.6995308303615,38.8125000027312,-105.5));
#7276=CARTESIAN_POINT('Ctrl Pts',(74.5997654151808,38.7500000027312,-74.5997654151808));
#7277=CARTESIAN_POINT('Ctrl Pts',(105.5,38.6875000027312,-43.6995308303616));
#7278=CARTESIAN_POINT('Ctrl Pts',(105.5,38.6250000027312,-1.29200237310046E-14));
#7279=CARTESIAN_POINT('Ctrl Pts',(105.5,38.5625000027312,43.6995308303615));
#7280=CARTESIAN_POINT('Ctrl Pts',(74.5997654151808,38.5000000027312,74.5997654151808));
#7281=CARTESIAN_POINT('Ctrl Pts',(43.6995308303616,38.4375000027312,105.5));
#7282=CARTESIAN_POINT('Ctrl Pts',(1.93800355965069E-14,38.3750000027312,
105.5));
#7283=CARTESIAN_POINT('Origin',(0.,105.,0.));
#7284=CARTESIAN_POINT('',(3.23000593275114E-15,40.3750000027312,105.5));
#7285=CARTESIAN_POINT('',(3.23000593275114E-15,40.25,105.5));
#7286=CARTESIAN_POINT('',(-1.29200237310046E-14,105.,105.5));
#7287=CARTESIAN_POINT('Ctrl Pts',(1.93800355965069E-14,40.25,105.5));
#7288=CARTESIAN_POINT('Ctrl Pts',(-43.6995308303616,40.1875,105.5));
#7289=CARTESIAN_POINT('Ctrl Pts',(-74.5997654151808,40.125,74.5997654151808));
#7290=CARTESIAN_POINT('Ctrl Pts',(-105.5,40.0625,43.6995308303616));
#7291=CARTESIAN_POINT('Ctrl Pts',(-105.5,40.,0.));
#7292=CARTESIAN_POINT('Ctrl Pts',(-105.5,39.9375,-43.6995308303615));
#7293=CARTESIAN_POINT('Ctrl Pts',(-74.5997654151808,39.875,-74.5997654151808));
#7294=CARTESIAN_POINT('Ctrl Pts',(-43.6995308303615,39.8125,-105.5));
#7295=CARTESIAN_POINT('Ctrl Pts',(-6.46001186550229E-15,39.75,-105.5));
#7296=CARTESIAN_POINT('Ctrl Pts',(43.6995308303615,39.6875,-105.5));
#7297=CARTESIAN_POINT('Ctrl Pts',(74.5997654151808,39.625,-74.5997654151808));
#7298=CARTESIAN_POINT('Ctrl Pts',(105.5,39.5625,-43.6995308303616));
#7299=CARTESIAN_POINT('Ctrl Pts',(105.5,39.5,-1.29200237310046E-14));
#7300=CARTESIAN_POINT('Ctrl Pts',(105.5,39.4375,43.6995308303615));
#7301=CARTESIAN_POINT('Ctrl Pts',(74.5997654151808,39.375,74.5997654151808));
#7302=CARTESIAN_POINT('Ctrl Pts',(43.6995308303616,39.3125,105.5));
#7303=CARTESIAN_POINT('Ctrl Pts',(1.93800355965069E-14,39.25,105.5));
#7304=CARTESIAN_POINT('Ctrl Pts',(1.93800355965069E-14,40.3750000027312,
105.5));
#7305=CARTESIAN_POINT('Ctrl Pts',(-43.6995308303616,40.3125000027312,105.5));
#7306=CARTESIAN_POINT('Ctrl Pts',(-74.5997654151808,40.2500000027312,74.5997654151808));
#7307=CARTESIAN_POINT('Ctrl Pts',(-105.5,40.1875000027312,43.6995308303616));
#7308=CARTESIAN_POINT('Ctrl Pts',(-105.5,40.1250000027312,0.));
#7309=CARTESIAN_POINT('Ctrl Pts',(-105.5,40.0625000027312,-43.6995308303615));
#7310=CARTESIAN_POINT('Ctrl Pts',(-74.5997654151808,40.0000000027312,-74.5997654151808));
#7311=CARTESIAN_POINT('Ctrl Pts',(-43.6995308303615,39.9375000027312,-105.5));
#7312=CARTESIAN_POINT('Ctrl Pts',(-6.46001186550229E-15,39.8750000027312,
-105.5));
#7313=CARTESIAN_POINT('Ctrl Pts',(43.6995308303615,39.8125000027312,-105.5));
#7314=CARTESIAN_POINT('Ctrl Pts',(74.5997654151808,39.7500000027312,-74.5997654151808));
#7315=CARTESIAN_POINT('Ctrl Pts',(105.5,39.6875000027312,-43.6995308303616));
#7316=CARTESIAN_POINT('Ctrl Pts',(105.5,39.6250000027312,-1.29200237310046E-14));
#7317=CARTESIAN_POINT('Ctrl Pts',(105.5,39.5625000027312,43.6995308303615));
#7318=CARTESIAN_POINT('Ctrl Pts',(74.5997654151808,39.5000000027312,74.5997654151808));
#7319=CARTESIAN_POINT('Ctrl Pts',(43.6995308303616,39.4375000027312,105.5));
#7320=CARTESIAN_POINT('Ctrl Pts',(1.93800355965069E-14,39.3750000027312,
105.5));
#7321=CARTESIAN_POINT('Origin',(0.,105.,0.));
#7322=CARTESIAN_POINT('',(3.23000593275114E-15,41.3750000027312,105.5));
#7323=CARTESIAN_POINT('',(3.23000593275114E-15,41.25,105.5));
#7324=CARTESIAN_POINT('',(-1.29200237310046E-14,105.,105.5));
#7325=CARTESIAN_POINT('Ctrl Pts',(1.93800355965069E-14,41.25,105.5));
#7326=CARTESIAN_POINT('Ctrl Pts',(-43.6995308303616,41.1875,105.5));
#7327=CARTESIAN_POINT('Ctrl Pts',(-74.5997654151808,41.125,74.5997654151808));
#7328=CARTESIAN_POINT('Ctrl Pts',(-105.5,41.0625,43.6995308303616));
#7329=CARTESIAN_POINT('Ctrl Pts',(-105.5,41.,0.));
#7330=CARTESIAN_POINT('Ctrl Pts',(-105.5,40.9375,-43.6995308303615));
#7331=CARTESIAN_POINT('Ctrl Pts',(-74.5997654151808,40.875,-74.5997654151808));
#7332=CARTESIAN_POINT('Ctrl Pts',(-43.6995308303615,40.8125,-105.5));
#7333=CARTESIAN_POINT('Ctrl Pts',(-6.46001186550229E-15,40.75,-105.5));
#7334=CARTESIAN_POINT('Ctrl Pts',(43.6995308303615,40.6875,-105.5));
#7335=CARTESIAN_POINT('Ctrl Pts',(74.5997654151808,40.625,-74.5997654151808));
#7336=CARTESIAN_POINT('Ctrl Pts',(105.5,40.5625,-43.6995308303616));
#7337=CARTESIAN_POINT('Ctrl Pts',(105.5,40.5,-1.29200237310046E-14));
#7338=CARTESIAN_POINT('Ctrl Pts',(105.5,40.4375,43.6995308303615));
#7339=CARTESIAN_POINT('Ctrl Pts',(74.5997654151808,40.375,74.5997654151808));
#7340=CARTESIAN_POINT('Ctrl Pts',(43.6995308303616,40.3125,105.5));
#7341=CARTESIAN_POINT('Ctrl Pts',(1.93800355965069E-14,40.25,105.5));
#7342=CARTESIAN_POINT('Ctrl Pts',(1.93800355965069E-14,41.3750000027312,
105.5));
#7343=CARTESIAN_POINT('Ctrl Pts',(-43.6995308303616,41.3125000027312,105.5));
#7344=CARTESIAN_POINT('Ctrl Pts',(-74.5997654151808,41.2500000027312,74.5997654151808));
#7345=CARTESIAN_POINT('Ctrl Pts',(-105.5,41.1875000027312,43.6995308303616));
#7346=CARTESIAN_POINT('Ctrl Pts',(-105.5,41.1250000027312,0.));
#7347=CARTESIAN_POINT('Ctrl Pts',(-105.5,41.0625000027312,-43.6995308303615));
#7348=CARTESIAN_POINT('Ctrl Pts',(-74.5997654151808,41.0000000027312,-74.5997654151808));
#7349=CARTESIAN_POINT('Ctrl Pts',(-43.6995308303615,40.9375000027312,-105.5));
#7350=CARTESIAN_POINT('Ctrl Pts',(-6.46001186550229E-15,40.8750000027312,
-105.5));
#7351=CARTESIAN_POINT('Ctrl Pts',(43.6995308303615,40.8125000027312,-105.5));
#7352=CARTESIAN_POINT('Ctrl Pts',(74.5997654151808,40.7500000027312,-74.5997654151808));
#7353=CARTESIAN_POINT('Ctrl Pts',(105.5,40.6875000027312,-43.6995308303616));
#7354=CARTESIAN_POINT('Ctrl Pts',(105.5,40.6250000027312,-1.29200237310046E-14));
#7355=CARTESIAN_POINT('Ctrl Pts',(105.5,40.5625000027312,43.6995308303615));
#7356=CARTESIAN_POINT('Ctrl Pts',(74.5997654151808,40.5000000027312,74.5997654151808));
#7357=CARTESIAN_POINT('Ctrl Pts',(43.6995308303616,40.4375000027312,105.5));
#7358=CARTESIAN_POINT('Ctrl Pts',(1.93800355965069E-14,40.3750000027312,
105.5));
#7359=CARTESIAN_POINT('Origin',(0.,105.,0.));
#7360=CARTESIAN_POINT('',(3.23000593275114E-15,42.3750000027312,105.5));
#7361=CARTESIAN_POINT('',(3.23000593275114E-15,42.25,105.5));
#7362=CARTESIAN_POINT('',(-1.29200237310046E-14,105.,105.5));
#7363=CARTESIAN_POINT('Ctrl Pts',(1.93800355965069E-14,42.25,105.5));
#7364=CARTESIAN_POINT('Ctrl Pts',(-43.6995308303616,42.1875,105.5));
#7365=CARTESIAN_POINT('Ctrl Pts',(-74.5997654151808,42.125,74.5997654151808));
#7366=CARTESIAN_POINT('Ctrl Pts',(-105.5,42.0625,43.6995308303616));
#7367=CARTESIAN_POINT('Ctrl Pts',(-105.5,42.,0.));
#7368=CARTESIAN_POINT('Ctrl Pts',(-105.5,41.9375,-43.6995308303615));
#7369=CARTESIAN_POINT('Ctrl Pts',(-74.5997654151808,41.875,-74.5997654151808));
#7370=CARTESIAN_POINT('Ctrl Pts',(-43.6995308303615,41.8125,-105.5));
#7371=CARTESIAN_POINT('Ctrl Pts',(-6.46001186550229E-15,41.75,-105.5));
#7372=CARTESIAN_POINT('Ctrl Pts',(43.6995308303615,41.6875,-105.5));
#7373=CARTESIAN_POINT('Ctrl Pts',(74.5997654151808,41.625,-74.5997654151808));
#7374=CARTESIAN_POINT('Ctrl Pts',(105.5,41.5625,-43.6995308303616));
#7375=CARTESIAN_POINT('Ctrl Pts',(105.5,41.5,-1.29200237310046E-14));
#7376=CARTESIAN_POINT('Ctrl Pts',(105.5,41.4375,43.6995308303615));
#7377=CARTESIAN_POINT('Ctrl Pts',(74.5997654151808,41.375,74.5997654151808));
#7378=CARTESIAN_POINT('Ctrl Pts',(43.6995308303616,41.3125,105.5));
#7379=CARTESIAN_POINT('Ctrl Pts',(1.93800355965069E-14,41.25,105.5));
#7380=CARTESIAN_POINT('Ctrl Pts',(1.93800355965069E-14,42.3750000027312,
105.5));
#7381=CARTESIAN_POINT('Ctrl Pts',(-43.6995308303616,42.3125000027312,105.5));
#7382=CARTESIAN_POINT('Ctrl Pts',(-74.5997654151808,42.2500000027312,74.5997654151808));
#7383=CARTESIAN_POINT('Ctrl Pts',(-105.5,42.1875000027312,43.6995308303616));
#7384=CARTESIAN_POINT('Ctrl Pts',(-105.5,42.1250000027312,0.));
#7385=CARTESIAN_POINT('Ctrl Pts',(-105.5,42.0625000027312,-43.6995308303615));
#7386=CARTESIAN_POINT('Ctrl Pts',(-74.5997654151808,42.0000000027312,-74.5997654151808));
#7387=CARTESIAN_POINT('Ctrl Pts',(-43.6995308303615,41.9375000027312,-105.5));
#7388=CARTESIAN_POINT('Ctrl Pts',(-6.46001186550229E-15,41.8750000027312,
-105.5));
#7389=CARTESIAN_POINT('Ctrl Pts',(43.6995308303615,41.8125000027312,-105.5));
#7390=CARTESIAN_POINT('Ctrl Pts',(74.5997654151808,41.7500000027312,-74.5997654151808));
#7391=CARTESIAN_POINT('Ctrl Pts',(105.5,41.6875000027312,-43.6995308303616));
#7392=CARTESIAN_POINT('Ctrl Pts',(105.5,41.6250000027312,-1.29200237310046E-14));
#7393=CARTESIAN_POINT('Ctrl Pts',(105.5,41.5625000027312,43.6995308303615));
#7394=CARTESIAN_POINT('Ctrl Pts',(74.5997654151808,41.5000000027312,74.5997654151808));
#7395=CARTESIAN_POINT('Ctrl Pts',(43.6995308303616,41.4375000027312,105.5));
#7396=CARTESIAN_POINT('Ctrl Pts',(1.93800355965069E-14,41.3750000027312,
105.5));
#7397=CARTESIAN_POINT('Origin',(0.,105.,0.));
#7398=CARTESIAN_POINT('',(3.23000593275114E-15,43.3750000027312,105.5));
#7399=CARTESIAN_POINT('',(3.23000593275114E-15,43.25,105.5));
#7400=CARTESIAN_POINT('',(-1.29200237310046E-14,105.,105.5));
#7401=CARTESIAN_POINT('Ctrl Pts',(1.93800355965069E-14,43.25,105.5));
#7402=CARTESIAN_POINT('Ctrl Pts',(-43.6995308303616,43.1875,105.5));
#7403=CARTESIAN_POINT('Ctrl Pts',(-74.5997654151808,43.125,74.5997654151808));
#7404=CARTESIAN_POINT('Ctrl Pts',(-105.5,43.0625,43.6995308303616));
#7405=CARTESIAN_POINT('Ctrl Pts',(-105.5,43.,0.));
#7406=CARTESIAN_POINT('Ctrl Pts',(-105.5,42.9375,-43.6995308303615));
#7407=CARTESIAN_POINT('Ctrl Pts',(-74.5997654151808,42.875,-74.5997654151808));
#7408=CARTESIAN_POINT('Ctrl Pts',(-43.6995308303615,42.8125,-105.5));
#7409=CARTESIAN_POINT('Ctrl Pts',(-6.46001186550229E-15,42.75,-105.5));
#7410=CARTESIAN_POINT('Ctrl Pts',(43.6995308303615,42.6875,-105.5));
#7411=CARTESIAN_POINT('Ctrl Pts',(74.5997654151808,42.625,-74.5997654151808));
#7412=CARTESIAN_POINT('Ctrl Pts',(105.5,42.5625,-43.6995308303616));
#7413=CARTESIAN_POINT('Ctrl Pts',(105.5,42.5,-1.29200237310046E-14));
#7414=CARTESIAN_POINT('Ctrl Pts',(105.5,42.4375,43.6995308303615));
#7415=CARTESIAN_POINT('Ctrl Pts',(74.5997654151808,42.375,74.5997654151808));
#7416=CARTESIAN_POINT('Ctrl Pts',(43.6995308303616,42.3125,105.5));
#7417=CARTESIAN_POINT('Ctrl Pts',(1.93800355965069E-14,42.25,105.5));
#7418=CARTESIAN_POINT('Ctrl Pts',(1.93800355965069E-14,43.3750000027312,
105.5));
#7419=CARTESIAN_POINT('Ctrl Pts',(-43.6995308303616,43.3125000027312,105.5));
#7420=CARTESIAN_POINT('Ctrl Pts',(-74.5997654151808,43.2500000027312,74.5997654151808));
#7421=CARTESIAN_POINT('Ctrl Pts',(-105.5,43.1875000027312,43.6995308303616));
#7422=CARTESIAN_POINT('Ctrl Pts',(-105.5,43.1250000027312,0.));
#7423=CARTESIAN_POINT('Ctrl Pts',(-105.5,43.0625000027312,-43.6995308303615));
#7424=CARTESIAN_POINT('Ctrl Pts',(-74.5997654151808,43.0000000027312,-74.5997654151808));
#7425=CARTESIAN_POINT('Ctrl Pts',(-43.6995308303615,42.9375000027312,-105.5));
#7426=CARTESIAN_POINT('Ctrl Pts',(-6.46001186550229E-15,42.8750000027312,
-105.5));
#7427=CARTESIAN_POINT('Ctrl Pts',(43.6995308303615,42.8125000027312,-105.5));
#7428=CARTESIAN_POINT('Ctrl Pts',(74.5997654151808,42.7500000027312,-74.5997654151808));
#7429=CARTESIAN_POINT('Ctrl Pts',(105.5,42.6875000027312,-43.6995308303616));
#7430=CARTESIAN_POINT('Ctrl Pts',(105.5,42.6250000027312,-1.29200237310046E-14));
#7431=CARTESIAN_POINT('Ctrl Pts',(105.5,42.5625000027312,43.6995308303615));
#7432=CARTESIAN_POINT('Ctrl Pts',(74.5997654151808,42.5000000027312,74.5997654151808));
#7433=CARTESIAN_POINT('Ctrl Pts',(43.6995308303616,42.4375000027312,105.5));
#7434=CARTESIAN_POINT('Ctrl Pts',(1.93800355965069E-14,42.3750000027312,
105.5));
#7435=CARTESIAN_POINT('Origin',(0.,105.,0.));
#7436=CARTESIAN_POINT('',(3.23000593275114E-15,44.3750000027312,105.5));
#7437=CARTESIAN_POINT('',(3.23000593275114E-15,44.25,105.5));
#7438=CARTESIAN_POINT('',(-1.29200237310046E-14,105.,105.5));
#7439=CARTESIAN_POINT('Ctrl Pts',(1.93800355965069E-14,44.25,105.5));
#7440=CARTESIAN_POINT('Ctrl Pts',(-43.6995308303616,44.1875,105.5));
#7441=CARTESIAN_POINT('Ctrl Pts',(-74.5997654151808,44.125,74.5997654151808));
#7442=CARTESIAN_POINT('Ctrl Pts',(-105.5,44.0625,43.6995308303616));
#7443=CARTESIAN_POINT('Ctrl Pts',(-105.5,44.,0.));
#7444=CARTESIAN_POINT('Ctrl Pts',(-105.5,43.9375,-43.6995308303615));
#7445=CARTESIAN_POINT('Ctrl Pts',(-74.5997654151808,43.875,-74.5997654151808));
#7446=CARTESIAN_POINT('Ctrl Pts',(-43.6995308303615,43.8125,-105.5));
#7447=CARTESIAN_POINT('Ctrl Pts',(-6.46001186550229E-15,43.75,-105.5));
#7448=CARTESIAN_POINT('Ctrl Pts',(43.6995308303615,43.6875,-105.5));
#7449=CARTESIAN_POINT('Ctrl Pts',(74.5997654151808,43.625,-74.5997654151808));
#7450=CARTESIAN_POINT('Ctrl Pts',(105.5,43.5625,-43.6995308303616));
#7451=CARTESIAN_POINT('Ctrl Pts',(105.5,43.5,-1.29200237310046E-14));
#7452=CARTESIAN_POINT('Ctrl Pts',(105.5,43.4375,43.6995308303615));
#7453=CARTESIAN_POINT('Ctrl Pts',(74.5997654151808,43.375,74.5997654151808));
#7454=CARTESIAN_POINT('Ctrl Pts',(43.6995308303616,43.3125,105.5));
#7455=CARTESIAN_POINT('Ctrl Pts',(1.93800355965069E-14,43.25,105.5));
#7456=CARTESIAN_POINT('Ctrl Pts',(1.93800355965069E-14,44.3750000027312,
105.5));
#7457=CARTESIAN_POINT('Ctrl Pts',(-43.6995308303616,44.3125000027312,105.5));
#7458=CARTESIAN_POINT('Ctrl Pts',(-74.5997654151808,44.2500000027312,74.5997654151808));
#7459=CARTESIAN_POINT('Ctrl Pts',(-105.5,44.1875000027312,43.6995308303616));
#7460=CARTESIAN_POINT('Ctrl Pts',(-105.5,44.1250000027312,0.));
#7461=CARTESIAN_POINT('Ctrl Pts',(-105.5,44.0625000027312,-43.6995308303615));
#7462=CARTESIAN_POINT('Ctrl Pts',(-74.5997654151808,44.0000000027312,-74.5997654151808));
#7463=CARTESIAN_POINT('Ctrl Pts',(-43.6995308303615,43.9375000027312,-105.5));
#7464=CARTESIAN_POINT('Ctrl Pts',(-6.46001186550229E-15,43.8750000027312,
-105.5));
#7465=CARTESIAN_POINT('Ctrl Pts',(43.6995308303615,43.8125000027312,-105.5));
#7466=CARTESIAN_POINT('Ctrl Pts',(74.5997654151808,43.7500000027312,-74.5997654151808));
#7467=CARTESIAN_POINT('Ctrl Pts',(105.5,43.6875000027312,-43.6995308303616));
#7468=CARTESIAN_POINT('Ctrl Pts',(105.5,43.6250000027312,-1.29200237310046E-14));
#7469=CARTESIAN_POINT('Ctrl Pts',(105.5,43.5625000027312,43.6995308303615));
#7470=CARTESIAN_POINT('Ctrl Pts',(74.5997654151808,43.5000000027312,74.5997654151808));
#7471=CARTESIAN_POINT('Ctrl Pts',(43.6995308303616,43.4375000027312,105.5));
#7472=CARTESIAN_POINT('Ctrl Pts',(1.93800355965069E-14,43.3750000027312,
105.5));
#7473=CARTESIAN_POINT('Origin',(0.,105.,0.));
#7474=CARTESIAN_POINT('',(3.23000593275114E-15,45.3750000027312,105.5));
#7475=CARTESIAN_POINT('',(3.23000593275114E-15,45.25,105.5));
#7476=CARTESIAN_POINT('',(-1.29200237310046E-14,105.,105.5));
#7477=CARTESIAN_POINT('Ctrl Pts',(1.93800355965069E-14,45.25,105.5));
#7478=CARTESIAN_POINT('Ctrl Pts',(-43.6995308303616,45.1875,105.5));
#7479=CARTESIAN_POINT('Ctrl Pts',(-74.5997654151808,45.125,74.5997654151808));
#7480=CARTESIAN_POINT('Ctrl Pts',(-105.5,45.0625,43.6995308303616));
#7481=CARTESIAN_POINT('Ctrl Pts',(-105.5,45.,0.));
#7482=CARTESIAN_POINT('Ctrl Pts',(-105.5,44.9375,-43.6995308303615));
#7483=CARTESIAN_POINT('Ctrl Pts',(-74.5997654151808,44.875,-74.5997654151808));
#7484=CARTESIAN_POINT('Ctrl Pts',(-43.6995308303615,44.8125,-105.5));
#7485=CARTESIAN_POINT('Ctrl Pts',(-6.46001186550229E-15,44.75,-105.5));
#7486=CARTESIAN_POINT('Ctrl Pts',(43.6995308303615,44.6875,-105.5));
#7487=CARTESIAN_POINT('Ctrl Pts',(74.5997654151808,44.625,-74.5997654151808));
#7488=CARTESIAN_POINT('Ctrl Pts',(105.5,44.5625,-43.6995308303616));
#7489=CARTESIAN_POINT('Ctrl Pts',(105.5,44.5,-1.29200237310046E-14));
#7490=CARTESIAN_POINT('Ctrl Pts',(105.5,44.4375,43.6995308303615));
#7491=CARTESIAN_POINT('Ctrl Pts',(74.5997654151808,44.375,74.5997654151808));
#7492=CARTESIAN_POINT('Ctrl Pts',(43.6995308303616,44.3125,105.5));
#7493=CARTESIAN_POINT('Ctrl Pts',(1.93800355965069E-14,44.25,105.5));
#7494=CARTESIAN_POINT('Ctrl Pts',(1.93800355965069E-14,45.3750000027312,
105.5));
#7495=CARTESIAN_POINT('Ctrl Pts',(-43.6995308303616,45.3125000027312,105.5));
#7496=CARTESIAN_POINT('Ctrl Pts',(-74.5997654151808,45.2500000027312,74.5997654151808));
#7497=CARTESIAN_POINT('Ctrl Pts',(-105.5,45.1875000027312,43.6995308303616));
#7498=CARTESIAN_POINT('Ctrl Pts',(-105.5,45.1250000027312,0.));
#7499=CARTESIAN_POINT('Ctrl Pts',(-105.5,45.0625000027312,-43.6995308303615));
#7500=CARTESIAN_POINT('Ctrl Pts',(-74.5997654151808,45.0000000027312,-74.5997654151808));
#7501=CARTESIAN_POINT('Ctrl Pts',(-43.6995308303615,44.9375000027312,-105.5));
#7502=CARTESIAN_POINT('Ctrl Pts',(-6.46001186550229E-15,44.8750000027312,
-105.5));
#7503=CARTESIAN_POINT('Ctrl Pts',(43.6995308303615,44.8125000027312,-105.5));
#7504=CARTESIAN_POINT('Ctrl Pts',(74.5997654151808,44.7500000027312,-74.5997654151808));
#7505=CARTESIAN_POINT('Ctrl Pts',(105.5,44.6875000027312,-43.6995308303616));
#7506=CARTESIAN_POINT('Ctrl Pts',(105.5,44.6250000027312,-1.29200237310046E-14));
#7507=CARTESIAN_POINT('Ctrl Pts',(105.5,44.5625000027312,43.6995308303615));
#7508=CARTESIAN_POINT('Ctrl Pts',(74.5997654151808,44.5000000027312,74.5997654151808));
#7509=CARTESIAN_POINT('Ctrl Pts',(43.6995308303616,44.4375000027312,105.5));
#7510=CARTESIAN_POINT('Ctrl Pts',(1.93800355965069E-14,44.3750000027312,
105.5));
#7511=CARTESIAN_POINT('Origin',(0.,105.,0.));
#7512=CARTESIAN_POINT('',(3.23000593275114E-15,46.3750000027312,105.5));
#7513=CARTESIAN_POINT('',(3.23000593275114E-15,46.25,105.5));
#7514=CARTESIAN_POINT('',(-1.29200237310046E-14,105.,105.5));
#7515=CARTESIAN_POINT('Ctrl Pts',(1.93800355965069E-14,46.25,105.5));
#7516=CARTESIAN_POINT('Ctrl Pts',(-43.6995308303616,46.1875,105.5));
#7517=CARTESIAN_POINT('Ctrl Pts',(-74.5997654151808,46.125,74.5997654151808));
#7518=CARTESIAN_POINT('Ctrl Pts',(-105.5,46.0625,43.6995308303616));
#7519=CARTESIAN_POINT('Ctrl Pts',(-105.5,46.,0.));
#7520=CARTESIAN_POINT('Ctrl Pts',(-105.5,45.9375,-43.6995308303615));
#7521=CARTESIAN_POINT('Ctrl Pts',(-74.5997654151808,45.875,-74.5997654151808));
#7522=CARTESIAN_POINT('Ctrl Pts',(-43.6995308303615,45.8125,-105.5));
#7523=CARTESIAN_POINT('Ctrl Pts',(-6.46001186550229E-15,45.75,-105.5));
#7524=CARTESIAN_POINT('Ctrl Pts',(43.6995308303615,45.6875,-105.5));
#7525=CARTESIAN_POINT('Ctrl Pts',(74.5997654151808,45.625,-74.5997654151808));
#7526=CARTESIAN_POINT('Ctrl Pts',(105.5,45.5625,-43.6995308303616));
#7527=CARTESIAN_POINT('Ctrl Pts',(105.5,45.5,-1.29200237310046E-14));
#7528=CARTESIAN_POINT('Ctrl Pts',(105.5,45.4375,43.6995308303615));
#7529=CARTESIAN_POINT('Ctrl Pts',(74.5997654151808,45.375,74.5997654151808));
#7530=CARTESIAN_POINT('Ctrl Pts',(43.6995308303616,45.3125,105.5));
#7531=CARTESIAN_POINT('Ctrl Pts',(1.93800355965069E-14,45.25,105.5));
#7532=CARTESIAN_POINT('Ctrl Pts',(1.93800355965069E-14,46.3750000027312,
105.5));
#7533=CARTESIAN_POINT('Ctrl Pts',(-43.6995308303616,46.3125000027312,105.5));
#7534=CARTESIAN_POINT('Ctrl Pts',(-74.5997654151808,46.2500000027312,74.5997654151808));
#7535=CARTESIAN_POINT('Ctrl Pts',(-105.5,46.1875000027312,43.6995308303616));
#7536=CARTESIAN_POINT('Ctrl Pts',(-105.5,46.1250000027312,0.));
#7537=CARTESIAN_POINT('Ctrl Pts',(-105.5,46.0625000027312,-43.6995308303615));
#7538=CARTESIAN_POINT('Ctrl Pts',(-74.5997654151808,46.0000000027312,-74.5997654151808));
#7539=CARTESIAN_POINT('Ctrl Pts',(-43.6995308303615,45.9375000027312,-105.5));
#7540=CARTESIAN_POINT('Ctrl Pts',(-6.46001186550229E-15,45.8750000027312,
-105.5));
#7541=CARTESIAN_POINT('Ctrl Pts',(43.6995308303615,45.8125000027312,-105.5));
#7542=CARTESIAN_POINT('Ctrl Pts',(74.5997654151808,45.7500000027312,-74.5997654151808));
#7543=CARTESIAN_POINT('Ctrl Pts',(105.5,45.6875000027312,-43.6995308303616));
#7544=CARTESIAN_POINT('Ctrl Pts',(105.5,45.6250000027312,-1.29200237310046E-14));
#7545=CARTESIAN_POINT('Ctrl Pts',(105.5,45.5625000027312,43.6995308303615));
#7546=CARTESIAN_POINT('Ctrl Pts',(74.5997654151808,45.5000000027312,74.5997654151808));
#7547=CARTESIAN_POINT('Ctrl Pts',(43.6995308303616,45.4375000027312,105.5));
#7548=CARTESIAN_POINT('Ctrl Pts',(1.93800355965069E-14,45.3750000027312,
105.5));
#7549=CARTESIAN_POINT('Origin',(0.,105.,0.));
#7550=CARTESIAN_POINT('',(3.23000593275114E-15,47.3750000027312,105.5));
#7551=CARTESIAN_POINT('',(3.23000593275114E-15,47.25,105.5));
#7552=CARTESIAN_POINT('',(-1.29200237310046E-14,105.,105.5));
#7553=CARTESIAN_POINT('Ctrl Pts',(1.93800355965069E-14,47.25,105.5));
#7554=CARTESIAN_POINT('Ctrl Pts',(-43.6995308303616,47.1875,105.5));
#7555=CARTESIAN_POINT('Ctrl Pts',(-74.5997654151808,47.125,74.5997654151808));
#7556=CARTESIAN_POINT('Ctrl Pts',(-105.5,47.0625,43.6995308303616));
#7557=CARTESIAN_POINT('Ctrl Pts',(-105.5,47.,0.));
#7558=CARTESIAN_POINT('Ctrl Pts',(-105.5,46.9375,-43.6995308303615));
#7559=CARTESIAN_POINT('Ctrl Pts',(-74.5997654151808,46.875,-74.5997654151808));
#7560=CARTESIAN_POINT('Ctrl Pts',(-43.6995308303615,46.8125,-105.5));
#7561=CARTESIAN_POINT('Ctrl Pts',(-6.46001186550229E-15,46.75,-105.5));
#7562=CARTESIAN_POINT('Ctrl Pts',(43.6995308303615,46.6875,-105.5));
#7563=CARTESIAN_POINT('Ctrl Pts',(74.5997654151808,46.625,-74.5997654151808));
#7564=CARTESIAN_POINT('Ctrl Pts',(105.5,46.5625,-43.6995308303616));
#7565=CARTESIAN_POINT('Ctrl Pts',(105.5,46.5,-1.29200237310046E-14));
#7566=CARTESIAN_POINT('Ctrl Pts',(105.5,46.4375,43.6995308303615));
#7567=CARTESIAN_POINT('Ctrl Pts',(74.5997654151808,46.375,74.5997654151808));
#7568=CARTESIAN_POINT('Ctrl Pts',(43.6995308303616,46.3125,105.5));
#7569=CARTESIAN_POINT('Ctrl Pts',(1.93800355965069E-14,46.25,105.5));
#7570=CARTESIAN_POINT('Ctrl Pts',(1.93800355965069E-14,47.3750000027312,
105.5));
#7571=CARTESIAN_POINT('Ctrl Pts',(-43.6995308303616,47.3125000027312,105.5));
#7572=CARTESIAN_POINT('Ctrl Pts',(-74.5997654151808,47.2500000027312,74.5997654151808));
#7573=CARTESIAN_POINT('Ctrl Pts',(-105.5,47.1875000027312,43.6995308303616));
#7574=CARTESIAN_POINT('Ctrl Pts',(-105.5,47.1250000027312,0.));
#7575=CARTESIAN_POINT('Ctrl Pts',(-105.5,47.0625000027312,-43.6995308303615));
#7576=CARTESIAN_POINT('Ctrl Pts',(-74.5997654151808,47.0000000027312,-74.5997654151808));
#7577=CARTESIAN_POINT('Ctrl Pts',(-43.6995308303615,46.9375000027312,-105.5));
#7578=CARTESIAN_POINT('Ctrl Pts',(-6.46001186550229E-15,46.8750000027312,
-105.5));
#7579=CARTESIAN_POINT('Ctrl Pts',(43.6995308303615,46.8125000027312,-105.5));
#7580=CARTESIAN_POINT('Ctrl Pts',(74.5997654151808,46.7500000027312,-74.5997654151808));
#7581=CARTESIAN_POINT('Ctrl Pts',(105.5,46.6875000027312,-43.6995308303616));
#7582=CARTESIAN_POINT('Ctrl Pts',(105.5,46.6250000027312,-1.29200237310046E-14));
#7583=CARTESIAN_POINT('Ctrl Pts',(105.5,46.5625000027312,43.6995308303615));
#7584=CARTESIAN_POINT('Ctrl Pts',(74.5997654151808,46.5000000027312,74.5997654151808));
#7585=CARTESIAN_POINT('Ctrl Pts',(43.6995308303616,46.4375000027312,105.5));
#7586=CARTESIAN_POINT('Ctrl Pts',(1.93800355965069E-14,46.3750000027312,
105.5));
#7587=CARTESIAN_POINT('Origin',(0.,105.,0.));
#7588=CARTESIAN_POINT('',(0.,100.,105.5));
#7589=CARTESIAN_POINT('Origin',(0.,100.,0.));
#7590=CARTESIAN_POINT('',(3.23000593275114E-15,49.25,105.5));
#7591=CARTESIAN_POINT('',(-1.29200237310046E-14,105.,105.5));
#7592=CARTESIAN_POINT('',(3.23000593275114E-15,48.25,105.5));
#7593=CARTESIAN_POINT('Ctrl Pts',(1.93800355965069E-14,49.25,105.5));
#7594=CARTESIAN_POINT('Ctrl Pts',(-43.6995308303616,49.1875,105.5));
#7595=CARTESIAN_POINT('Ctrl Pts',(-74.5997654151808,49.125,74.5997654151808));
#7596=CARTESIAN_POINT('Ctrl Pts',(-105.5,49.0625,43.6995308303616));
#7597=CARTESIAN_POINT('Ctrl Pts',(-105.5,49.,0.));
#7598=CARTESIAN_POINT('Ctrl Pts',(-105.5,48.9375,-43.6995308303615));
#7599=CARTESIAN_POINT('Ctrl Pts',(-74.5997654151808,48.875,-74.5997654151808));
#7600=CARTESIAN_POINT('Ctrl Pts',(-43.6995308303615,48.8125,-105.5));
#7601=CARTESIAN_POINT('Ctrl Pts',(-6.46001186550229E-15,48.75,-105.5));
#7602=CARTESIAN_POINT('Ctrl Pts',(43.6995308303615,48.6875,-105.5));
#7603=CARTESIAN_POINT('Ctrl Pts',(74.5997654151808,48.625,-74.5997654151808));
#7604=CARTESIAN_POINT('Ctrl Pts',(105.5,48.5625,-43.6995308303616));
#7605=CARTESIAN_POINT('Ctrl Pts',(105.5,48.5,-1.29200237310046E-14));
#7606=CARTESIAN_POINT('Ctrl Pts',(105.5,48.4375,43.6995308303615));
#7607=CARTESIAN_POINT('Ctrl Pts',(74.5997654151808,48.375,74.5997654151808));
#7608=CARTESIAN_POINT('Ctrl Pts',(43.6995308303616,48.3125,105.5));
#7609=CARTESIAN_POINT('Ctrl Pts',(1.93800355965069E-14,48.25,105.5));
#7610=CARTESIAN_POINT('',(3.23000593275114E-15,48.3750000027312,105.5));
#7611=CARTESIAN_POINT('',(-1.29200237310046E-14,105.,105.5));
#7612=CARTESIAN_POINT('',(-105.5,49.1250000027312,0.));
#7613=CARTESIAN_POINT('Ctrl Pts',(-105.5,49.1250000027312,0.));
#7614=CARTESIAN_POINT('Ctrl Pts',(-105.5,49.0625000027312,-43.6995308303615));
#7615=CARTESIAN_POINT('Ctrl Pts',(-74.5997654151808,49.0000000027312,-74.5997654151808));
#7616=CARTESIAN_POINT('Ctrl Pts',(-43.6995308303615,48.9375000027312,-105.5));
#7617=CARTESIAN_POINT('Ctrl Pts',(-6.46001186550229E-15,48.8750000027312,
-105.5));
#7618=CARTESIAN_POINT('Ctrl Pts',(43.6995308303615,48.8125000027312,-105.5));
#7619=CARTESIAN_POINT('Ctrl Pts',(74.5997654151808,48.7500000027312,-74.5997654151808));
#7620=CARTESIAN_POINT('Ctrl Pts',(105.5,48.6875000027312,-43.6995308303616));
#7621=CARTESIAN_POINT('Ctrl Pts',(105.5,48.6250000027312,-1.29200237310046E-14));
#7622=CARTESIAN_POINT('Ctrl Pts',(105.5,48.5625000027312,43.6995308303615));
#7623=CARTESIAN_POINT('Ctrl Pts',(74.5997654151808,48.5000000027312,74.5997654151808));
#7624=CARTESIAN_POINT('Ctrl Pts',(43.6995308303616,48.4375000027312,105.5));
#7625=CARTESIAN_POINT('Ctrl Pts',(1.93800355965069E-14,48.3750000027312,
105.5));
#7626=CARTESIAN_POINT('',(-105.5,50.,0.));
#7627=CARTESIAN_POINT('',(-105.5,50.,0.));
#7628=CARTESIAN_POINT('Ctrl Pts',(-105.5,50.,0.));
#7629=CARTESIAN_POINT('Ctrl Pts',(-105.5,49.9375,-43.6995308303615));
#7630=CARTESIAN_POINT('Ctrl Pts',(-74.5997654151808,49.875,-74.5997654151808));
#7631=CARTESIAN_POINT('Ctrl Pts',(-43.6995308303615,49.8125,-105.5));
#7632=CARTESIAN_POINT('Ctrl Pts',(-6.46001186550229E-15,49.75,-105.5));
#7633=CARTESIAN_POINT('Ctrl Pts',(43.6995308303615,49.6875,-105.5));
#7634=CARTESIAN_POINT('Ctrl Pts',(74.5997654151808,49.625,-74.5997654151808));
#7635=CARTESIAN_POINT('Ctrl Pts',(105.5,49.5625,-43.6995308303616));
#7636=CARTESIAN_POINT('Ctrl Pts',(105.5,49.5,-1.29200237310046E-14));
#7637=CARTESIAN_POINT('Ctrl Pts',(105.5,49.4375,43.6995308303615));
#7638=CARTESIAN_POINT('Ctrl Pts',(74.5997654151808,49.375,74.5997654151808));
#7639=CARTESIAN_POINT('Ctrl Pts',(43.6995308303616,49.3125,105.5));
#7640=CARTESIAN_POINT('Ctrl Pts',(1.93800355965069E-14,49.25,105.5));
#7641=CARTESIAN_POINT('Origin',(0.,105.,0.));
#7642=CARTESIAN_POINT('',(0.,10.0000000000002,120.5));
#7643=CARTESIAN_POINT('',(-1.47569939297256E-14,10.0000000000002,-120.5));
#7644=CARTESIAN_POINT('Origin',(0.,10.0000000000002,0.));
#7645=CARTESIAN_POINT('Origin',(0.,10.0000000000002,0.));
#7646=CARTESIAN_POINT('',(0.,100.,120.5));
#7647=CARTESIAN_POINT('',(-1.47569939297256E-14,105.,120.5));
#7648=CARTESIAN_POINT('Origin',(0.,100.,0.));
#7649=CARTESIAN_POINT('',(120.084345357753,50.,9.99999999999999));
#7650=CARTESIAN_POINT('',(120.084345357753,50.,-9.99999999999999));
#7651=CARTESIAN_POINT('Ctrl Pts',(120.084345357753,50.,9.99999999999999));
#7652=CARTESIAN_POINT('Ctrl Pts',(120.084345357753,48.7437566650744,9.99999999999999));
#7653=CARTESIAN_POINT('Ctrl Pts',(120.10608848982,47.4041746217151,9.74882112932349));
#7654=CARTESIAN_POINT('Ctrl Pts',(120.184575491108,44.9405529209964,8.72810511950586));
#7655=CARTESIAN_POINT('Ctrl Pts',(120.240180997842,43.816464013271,7.95859963700194));
#7656=CARTESIAN_POINT('Ctrl Pts',(120.344523336394,42.0414017916464,6.18353741537737));
#7657=CARTESIAN_POINT('Ctrl Pts',(120.400045183931,41.2718952010862,5.05944787646731));
#7658=CARTESIAN_POINT('Ctrl Pts',(120.478340752227,40.2511783443158,2.59582408417372));
#7659=CARTESIAN_POINT('Ctrl Pts',(120.5,40.,1.25624131276716));
#7660=CARTESIAN_POINT('Ctrl Pts',(120.5,40.,-1.25624131276716));
#7661=CARTESIAN_POINT('Ctrl Pts',(120.478340752227,40.2511783443158,-2.59582408417371));
#7662=CARTESIAN_POINT('Ctrl Pts',(120.400045183931,41.2718952010862,-5.05944787646731));
#7663=CARTESIAN_POINT('Ctrl Pts',(120.344523336394,42.0414017916464,-6.18353741537737));
#7664=CARTESIAN_POINT('Ctrl Pts',(120.240180997842,43.816464013271,-7.95859963700194));
#7665=CARTESIAN_POINT('Ctrl Pts',(120.184575491108,44.9405529209964,-8.72810511950586));
#7666=CARTESIAN_POINT('Ctrl Pts',(120.10608848982,47.4041746217151,-9.74882112932349));
#7667=CARTESIAN_POINT('Ctrl Pts',(120.084345357753,48.7437566650744,-9.99999999999999));
#7668=CARTESIAN_POINT('Ctrl Pts',(120.084345357753,50.,-9.99999999999999));
#7669=CARTESIAN_POINT('Ctrl Pts',(120.084345357753,50.,-9.99999999999999));
#7670=CARTESIAN_POINT('Ctrl Pts',(120.084345357753,51.2562433349256,-9.99999999999999));
#7671=CARTESIAN_POINT('Ctrl Pts',(120.10608848982,52.5958253782849,-9.74882112932349));
#7672=CARTESIAN_POINT('Ctrl Pts',(120.184575491108,55.0594470790036,-8.72810511950586));
#7673=CARTESIAN_POINT('Ctrl Pts',(120.240180997842,56.183535986729,-7.95859963700194));
#7674=CARTESIAN_POINT('Ctrl Pts',(120.344523336394,57.9585982083536,-6.18353741537737));
#7675=CARTESIAN_POINT('Ctrl Pts',(120.400045183931,58.7281047989138,-5.05944787646731));
#7676=CARTESIAN_POINT('Ctrl Pts',(120.478340752227,59.7488216556842,-2.59582408417371));
#7677=CARTESIAN_POINT('Ctrl Pts',(120.5,60.,-1.25624131276716));
#7678=CARTESIAN_POINT('Ctrl Pts',(120.5,60.,1.25624131276716));
#7679=CARTESIAN_POINT('Ctrl Pts',(120.478340752227,59.7488216556842,2.59582408417372));
#7680=CARTESIAN_POINT('Ctrl Pts',(120.400045183931,58.7281047989138,5.05944787646731));
#7681=CARTESIAN_POINT('Ctrl Pts',(120.344523336394,57.9585982083536,6.18353741537737));
#7682=CARTESIAN_POINT('Ctrl Pts',(120.240180997842,56.183535986729,7.95859963700194));
#7683=CARTESIAN_POINT('Ctrl Pts',(120.184575491108,55.0594470790036,8.72810511950586));
#7684=CARTESIAN_POINT('Ctrl Pts',(120.10608848982,52.5958253782849,9.74882112932349));
#7685=CARTESIAN_POINT('Ctrl Pts',(120.084345357753,51.2562433349256,9.99999999999999));
#7686=CARTESIAN_POINT('Ctrl Pts',(120.084345357753,50.,9.99999999999999));
#7687=CARTESIAN_POINT('',(-120.084345357753,50.,9.99999999999999));
#7688=CARTESIAN_POINT('',(-120.084345357753,50.,-9.99999999999999));
#7689=CARTESIAN_POINT('Ctrl Pts',(-120.084345357753,50.,9.99999999999999));
#7690=CARTESIAN_POINT('Ctrl Pts',(-120.084345357753,51.2562433349256,9.99999999999999));
#7691=CARTESIAN_POINT('Ctrl Pts',(-120.10608848982,52.5958253782849,9.74882112932349));
#7692=CARTESIAN_POINT('Ctrl Pts',(-120.184575491108,55.0594470790036,8.72810511950586));
#7693=CARTESIAN_POINT('Ctrl Pts',(-120.240180997842,56.183535986729,7.95859963700195));
#7694=CARTESIAN_POINT('Ctrl Pts',(-120.344523336394,57.9585982083536,6.18353741537737));
#7695=CARTESIAN_POINT('Ctrl Pts',(-120.400045183931,58.7281047989138,5.05944787646732));
#7696=CARTESIAN_POINT('Ctrl Pts',(-120.478340752227,59.7488216556842,2.59582408417372));
#7697=CARTESIAN_POINT('Ctrl Pts',(-120.5,60.,1.25624131276716));
#7698=CARTESIAN_POINT('Ctrl Pts',(-120.5,60.,-1.25624131276716));
#7699=CARTESIAN_POINT('Ctrl Pts',(-120.478340752227,59.7488216556842,-2.59582408417371));
#7700=CARTESIAN_POINT('Ctrl Pts',(-120.400045183931,58.7281047989138,-5.05944787646731));
#7701=CARTESIAN_POINT('Ctrl Pts',(-120.344523336394,57.9585982083536,-6.18353741537737));
#7702=CARTESIAN_POINT('Ctrl Pts',(-120.240180997842,56.183535986729,-7.95859963700194));
#7703=CARTESIAN_POINT('Ctrl Pts',(-120.184575491108,55.0594470790036,-8.72810511950586));
#7704=CARTESIAN_POINT('Ctrl Pts',(-120.10608848982,52.5958253782849,-9.74882112932349));
#7705=CARTESIAN_POINT('Ctrl Pts',(-120.084345357753,51.2562433349256,-9.99999999999999));
#7706=CARTESIAN_POINT('Ctrl Pts',(-120.084345357753,50.,-9.99999999999999));
#7707=CARTESIAN_POINT('Ctrl Pts',(-120.084345357753,50.,-9.99999999999999));
#7708=CARTESIAN_POINT('Ctrl Pts',(-120.084345357753,48.7437566650744,-9.99999999999999));
#7709=CARTESIAN_POINT('Ctrl Pts',(-120.10608848982,47.4041746217151,-9.74882112932349));
#7710=CARTESIAN_POINT('Ctrl Pts',(-120.184575491108,44.9405529209964,-8.72810511950586));
#7711=CARTESIAN_POINT('Ctrl Pts',(-120.240180997842,43.816464013271,-7.95859963700195));
#7712=CARTESIAN_POINT('Ctrl Pts',(-120.344523336394,42.0414017916464,-6.18353741537737));
#7713=CARTESIAN_POINT('Ctrl Pts',(-120.400045183931,41.2718952010862,-5.0594478764673));
#7714=CARTESIAN_POINT('Ctrl Pts',(-120.478340752227,40.2511783443158,-2.59582408417371));
#7715=CARTESIAN_POINT('Ctrl Pts',(-120.5,40.,-1.25624131276716));
#7716=CARTESIAN_POINT('Ctrl Pts',(-120.5,40.,1.25624131276716));
#7717=CARTESIAN_POINT('Ctrl Pts',(-120.478340752227,40.2511783443158,2.59582408417371));
#7718=CARTESIAN_POINT('Ctrl Pts',(-120.400045183931,41.2718952010862,5.05944787646731));
#7719=CARTESIAN_POINT('Ctrl Pts',(-120.344523336394,42.0414017916464,6.18353741537737));
#7720=CARTESIAN_POINT('Ctrl Pts',(-120.240180997842,43.816464013271,7.95859963700194));
#7721=CARTESIAN_POINT('Ctrl Pts',(-120.184575491108,44.9405529209964,8.72810511950586));
#7722=CARTESIAN_POINT('Ctrl Pts',(-120.10608848982,47.4041746217151,9.74882112932349));
#7723=CARTESIAN_POINT('Ctrl Pts',(-120.084345357753,48.7437566650744,9.99999999999999));
#7724=CARTESIAN_POINT('Ctrl Pts',(-120.084345357753,50.,9.99999999999999));
#7725=CARTESIAN_POINT('Origin',(0.,105.,0.));
#7726=CARTESIAN_POINT('Ctrl Pts',(1.93800355965069E-14,48.25,105.5));
#7727=CARTESIAN_POINT('Ctrl Pts',(-43.6995308303616,48.1875,105.5));
#7728=CARTESIAN_POINT('Ctrl Pts',(-74.5997654151808,48.125,74.5997654151808));
#7729=CARTESIAN_POINT('Ctrl Pts',(-105.5,48.0625,43.6995308303616));
#7730=CARTESIAN_POINT('Ctrl Pts',(-105.5,48.,0.));
#7731=CARTESIAN_POINT('Ctrl Pts',(-105.5,47.9375,-43.6995308303615));
#7732=CARTESIAN_POINT('Ctrl Pts',(-74.5997654151808,47.875,-74.5997654151808));
#7733=CARTESIAN_POINT('Ctrl Pts',(-43.6995308303615,47.8125,-105.5));
#7734=CARTESIAN_POINT('Ctrl Pts',(-6.46001186550229E-15,47.75,-105.5));
#7735=CARTESIAN_POINT('Ctrl Pts',(43.6995308303615,47.6875,-105.5));
#7736=CARTESIAN_POINT('Ctrl Pts',(74.5997654151808,47.625,-74.5997654151808));
#7737=CARTESIAN_POINT('Ctrl Pts',(105.5,47.5625,-43.6995308303616));
#7738=CARTESIAN_POINT('Ctrl Pts',(105.5,47.5,-1.29200237310046E-14));
#7739=CARTESIAN_POINT('Ctrl Pts',(105.5,47.4375,43.6995308303615));
#7740=CARTESIAN_POINT('Ctrl Pts',(74.5997654151808,47.375,74.5997654151808));
#7741=CARTESIAN_POINT('Ctrl Pts',(43.6995308303616,47.3125,105.5));
#7742=CARTESIAN_POINT('Ctrl Pts',(1.93800355965069E-14,47.25,105.5));
#7743=CARTESIAN_POINT('Ctrl Pts',(1.93800355965069E-14,48.3750000027312,
105.5));
#7744=CARTESIAN_POINT('Ctrl Pts',(-43.6995308303616,48.3125000027312,105.5));
#7745=CARTESIAN_POINT('Ctrl Pts',(-74.5997654151808,48.2500000027312,74.5997654151808));
#7746=CARTESIAN_POINT('Ctrl Pts',(-105.5,48.1875000027312,43.6995308303616));
#7747=CARTESIAN_POINT('Ctrl Pts',(-105.5,48.1250000027312,0.));
#7748=CARTESIAN_POINT('Ctrl Pts',(-105.5,48.0625000027312,-43.6995308303615));
#7749=CARTESIAN_POINT('Ctrl Pts',(-74.5997654151808,48.0000000027312,-74.5997654151808));
#7750=CARTESIAN_POINT('Ctrl Pts',(-43.6995308303615,47.9375000027312,-105.5));
#7751=CARTESIAN_POINT('Ctrl Pts',(-6.46001186550229E-15,47.8750000027312,
-105.5));
#7752=CARTESIAN_POINT('Ctrl Pts',(43.6995308303615,47.8125000027312,-105.5));
#7753=CARTESIAN_POINT('Ctrl Pts',(74.5997654151808,47.7500000027312,-74.5997654151808));
#7754=CARTESIAN_POINT('Ctrl Pts',(105.5,47.6875000027312,-43.6995308303616));
#7755=CARTESIAN_POINT('Ctrl Pts',(105.5,47.6250000027312,-1.29200237310046E-14));
#7756=CARTESIAN_POINT('Ctrl Pts',(105.5,47.5625000027312,43.6995308303615));
#7757=CARTESIAN_POINT('Ctrl Pts',(74.5997654151808,47.5000000027312,74.5997654151808));
#7758=CARTESIAN_POINT('Ctrl Pts',(43.6995308303616,47.4375000027312,105.5));
#7759=CARTESIAN_POINT('Ctrl Pts',(1.93800355965069E-14,47.3750000027312,
105.5));
#7760=CARTESIAN_POINT('Origin',(0.,105.,0.));
#7761=CARTESIAN_POINT('',(0.,105.,118.168461709225));
#7762=CARTESIAN_POINT('Origin',(0.,105.,0.));
#7763=CARTESIAN_POINT('',(-1.41446705301519E-14,105.,-115.5));
#7764=CARTESIAN_POINT('Origin',(0.,105.,0.));
#7765=CARTESIAN_POINT('Origin',(0.,0.,0.));
#7766=CARTESIAN_POINT('',(-1.40499437705757E-14,6.66133814775094E-15,-114.726497308104));
#7767=CARTESIAN_POINT('Origin',(0.,0.,0.));
#7768=CARTESIAN_POINT('Origin',(0.,0.,0.));
#7769=CARTESIAN_POINT('Origin',(0.,100.,0.));
#7770=CARTESIAN_POINT('',(-1.4058614088468E-14,100.,-114.797295826488));
#7771=CARTESIAN_POINT('Origin',(0.,100.,0.));
#7772=CARTESIAN_POINT('Origin',(0.,105.,0.));
#7773=CARTESIAN_POINT('',(-1.44714628392369E-14,105.,118.168461709225));
#7774=CARTESIAN_POINT('Origin',(-105.2293670625,49.8437500006828,0.));
#7775=CARTESIAN_POINT('',(-104.958734125,49.6875000013656,0.));
#7776=CARTESIAN_POINT('',(-105.5,49.1250000027312,0.));
#7777=CARTESIAN_POINT('Origin',(-105.2293670625,-0.156249999317216,0.));
#7778=CARTESIAN_POINT('',(-105.5,-1.04083408558608E-14,0.));
#7779=CARTESIAN_POINT('',(-105.5,-0.874999997268824,0.));
#7780=CARTESIAN_POINT('',(-104.958734125,-0.562499998634419,0.));
#7781=CARTESIAN_POINT('',(-105.5,-0.874999997268824,0.));
#7782=CARTESIAN_POINT('Ctrl Pts',(-104.958734125,49.6875000013656,0.));
#7783=CARTESIAN_POINT('Ctrl Pts',(-104.958734125,49.6250000013656,-43.4753311640868));
#7784=CARTESIAN_POINT('Ctrl Pts',(-74.2170326445434,49.5625000013656,-74.2170326445434));
#7785=CARTESIAN_POINT('Ctrl Pts',(-43.4753311640868,49.5000000013656,-104.958734125));
#7786=CARTESIAN_POINT('Ctrl Pts',(-6.42686888943697E-15,49.4375000013656,
-104.958734125));
#7787=CARTESIAN_POINT('Ctrl Pts',(43.4753311640868,49.3750000013656,-104.958734125));
#7788=CARTESIAN_POINT('Ctrl Pts',(74.2170326445434,49.3125000013656,-74.2170326445434));
#7789=CARTESIAN_POINT('Ctrl Pts',(104.958734125,49.2500000013656,-43.4753311640868));
#7790=CARTESIAN_POINT('Ctrl Pts',(104.958734125,49.1875000013656,-1.28537377788739E-14));
#7791=CARTESIAN_POINT('Ctrl Pts',(104.958734125,49.1250000013656,43.4753311640868));
#7792=CARTESIAN_POINT('Ctrl Pts',(74.2170326445434,49.0625000013656,74.2170326445434));
#7793=CARTESIAN_POINT('Ctrl Pts',(43.4753311640869,49.0000000013656,104.958734125));
#7794=CARTESIAN_POINT('Ctrl Pts',(1.92806066683109E-14,48.9375000013656,
104.958734125));
#7795=CARTESIAN_POINT('Ctrl Pts',(-43.4753311640868,48.8750000013656,104.958734125));
#7796=CARTESIAN_POINT('Ctrl Pts',(-74.2170326445434,48.8125000013656,74.2170326445434));
#7797=CARTESIAN_POINT('Ctrl Pts',(-104.958734125,48.7500000013656,43.4753311640869));
#7798=CARTESIAN_POINT('Ctrl Pts',(-104.958734125,48.6875000013656,0.));
#7799=CARTESIAN_POINT('Ctrl Pts',(-104.958734125,48.6250000013656,-43.4753311640868));
#7800=CARTESIAN_POINT('Ctrl Pts',(-74.2170326445434,48.5625000013656,-74.2170326445434));
#7801=CARTESIAN_POINT('Ctrl Pts',(-43.4753311640868,48.5000000013656,-104.958734125));
#7802=CARTESIAN_POINT('Ctrl Pts',(-6.42686888943697E-15,48.4375000013656,
-104.958734125));
#7803=CARTESIAN_POINT('Ctrl Pts',(43.4753311640868,48.3750000013656,-104.958734125));
#7804=CARTESIAN_POINT('Ctrl Pts',(74.2170326445434,48.3125000013656,-74.2170326445434));
#7805=CARTESIAN_POINT('Ctrl Pts',(104.958734125,48.2500000013656,-43.4753311640868));
#7806=CARTESIAN_POINT('Ctrl Pts',(104.958734125,48.1875000013656,-1.28537377788739E-14));
#7807=CARTESIAN_POINT('Ctrl Pts',(104.958734125,48.1250000013656,43.4753311640868));
#7808=CARTESIAN_POINT('Ctrl Pts',(74.2170326445434,48.0625000013656,74.2170326445434));
#7809=CARTESIAN_POINT('Ctrl Pts',(43.4753311640869,48.0000000013656,104.958734125));
#7810=CARTESIAN_POINT('Ctrl Pts',(1.92806066683109E-14,47.9375000013656,
104.958734125));
#7811=CARTESIAN_POINT('Ctrl Pts',(-43.4753311640868,47.8750000013656,104.958734125));
#7812=CARTESIAN_POINT('Ctrl Pts',(-74.2170326445434,47.8125000013656,74.2170326445434));
#7813=CARTESIAN_POINT('Ctrl Pts',(-104.958734125,47.7500000013656,43.4753311640869));
#7814=CARTESIAN_POINT('Ctrl Pts',(-104.958734125,47.6875000013656,0.));
#7815=CARTESIAN_POINT('Ctrl Pts',(-104.958734125,47.6250000013656,-43.4753311640868));
#7816=CARTESIAN_POINT('Ctrl Pts',(-74.2170326445434,47.5625000013656,-74.2170326445434));
#7817=CARTESIAN_POINT('Ctrl Pts',(-43.4753311640868,47.5000000013656,-104.958734125));
#7818=CARTESIAN_POINT('Ctrl Pts',(-6.42686888943697E-15,47.4375000013656,
-104.958734125));
#7819=CARTESIAN_POINT('Ctrl Pts',(43.4753311640868,47.3750000013656,-104.958734125));
#7820=CARTESIAN_POINT('Ctrl Pts',(74.2170326445434,47.3125000013656,-74.2170326445434));
#7821=CARTESIAN_POINT('Ctrl Pts',(104.958734125,47.2500000013656,-43.4753311640868));
#7822=CARTESIAN_POINT('Ctrl Pts',(104.958734125,47.1875000013656,-1.28537377788739E-14));
#7823=CARTESIAN_POINT('Ctrl Pts',(104.958734125,47.1250000013656,43.4753311640868));
#7824=CARTESIAN_POINT('Ctrl Pts',(74.2170326445434,47.0625000013656,74.2170326445434));
#7825=CARTESIAN_POINT('Ctrl Pts',(43.4753311640869,47.0000000013656,104.958734125));
#7826=CARTESIAN_POINT('Ctrl Pts',(1.92806066683109E-14,46.9375000013656,
104.958734125));
#7827=CARTESIAN_POINT('Ctrl Pts',(-43.4753311640868,46.8750000013656,104.958734125));
#7828=CARTESIAN_POINT('Ctrl Pts',(-74.2170326445434,46.8125000013656,74.2170326445434));
#7829=CARTESIAN_POINT('Ctrl Pts',(-104.958734125,46.7500000013656,43.4753311640869));
#7830=CARTESIAN_POINT('Ctrl Pts',(-104.958734125,46.6875000013656,0.));
#7831=CARTESIAN_POINT('Ctrl Pts',(-104.958734125,46.6250000013656,-43.4753311640868));
#7832=CARTESIAN_POINT('Ctrl Pts',(-74.2170326445434,46.5625000013656,-74.2170326445434));
#7833=CARTESIAN_POINT('Ctrl Pts',(-43.4753311640868,46.5000000013656,-104.958734125));
#7834=CARTESIAN_POINT('Ctrl Pts',(-6.42686888943697E-15,46.4375000013656,
-104.958734125));
#7835=CARTESIAN_POINT('Ctrl Pts',(43.4753311640868,46.3750000013656,-104.958734125));
#7836=CARTESIAN_POINT('Ctrl Pts',(74.2170326445434,46.3125000013656,-74.2170326445434));
#7837=CARTESIAN_POINT('Ctrl Pts',(104.958734125,46.2500000013656,-43.4753311640868));
#7838=CARTESIAN_POINT('Ctrl Pts',(104.958734125,46.1875000013656,-1.28537377788739E-14));
#7839=CARTESIAN_POINT('Ctrl Pts',(104.958734125,46.1250000013656,43.4753311640868));
#7840=CARTESIAN_POINT('Ctrl Pts',(74.2170326445434,46.0625000013656,74.2170326445434));
#7841=CARTESIAN_POINT('Ctrl Pts',(43.4753311640869,46.0000000013656,104.958734125));
#7842=CARTESIAN_POINT('Ctrl Pts',(1.92806066683109E-14,45.9375000013656,
104.958734125));
#7843=CARTESIAN_POINT('Ctrl Pts',(-43.4753311640868,45.8750000013656,104.958734125));
#7844=CARTESIAN_POINT('Ctrl Pts',(-74.2170326445434,45.8125000013656,74.2170326445434));
#7845=CARTESIAN_POINT('Ctrl Pts',(-104.958734125,45.7500000013656,43.4753311640869));
#7846=CARTESIAN_POINT('Ctrl Pts',(-104.958734125,45.6875000013656,0.));
#7847=CARTESIAN_POINT('Ctrl Pts',(-104.958734125,45.6250000013656,-43.4753311640868));
#7848=CARTESIAN_POINT('Ctrl Pts',(-74.2170326445434,45.5625000013656,-74.2170326445434));
#7849=CARTESIAN_POINT('Ctrl Pts',(-43.4753311640868,45.5000000013656,-104.958734125));
#7850=CARTESIAN_POINT('Ctrl Pts',(-6.42686888943697E-15,45.4375000013656,
-104.958734125));
#7851=CARTESIAN_POINT('Ctrl Pts',(43.4753311640868,45.3750000013656,-104.958734125));
#7852=CARTESIAN_POINT('Ctrl Pts',(74.2170326445434,45.3125000013656,-74.2170326445434));
#7853=CARTESIAN_POINT('Ctrl Pts',(104.958734125,45.2500000013656,-43.4753311640868));
#7854=CARTESIAN_POINT('Ctrl Pts',(104.958734125,45.1875000013656,-1.28537377788739E-14));
#7855=CARTESIAN_POINT('Ctrl Pts',(104.958734125,45.1250000013656,43.4753311640868));
#7856=CARTESIAN_POINT('Ctrl Pts',(74.2170326445434,45.0625000013656,74.2170326445434));
#7857=CARTESIAN_POINT('Ctrl Pts',(43.4753311640869,45.0000000013656,104.958734125));
#7858=CARTESIAN_POINT('Ctrl Pts',(1.92806066683109E-14,44.9375000013656,
104.958734125));
#7859=CARTESIAN_POINT('Ctrl Pts',(-43.4753311640868,44.8750000013656,104.958734125));
#7860=CARTESIAN_POINT('Ctrl Pts',(-74.2170326445434,44.8125000013656,74.2170326445434));
#7861=CARTESIAN_POINT('Ctrl Pts',(-104.958734125,44.7500000013656,43.4753311640869));
#7862=CARTESIAN_POINT('Ctrl Pts',(-104.958734125,44.6875000013656,0.));
#7863=CARTESIAN_POINT('Ctrl Pts',(-104.958734125,44.6250000013656,-43.4753311640868));
#7864=CARTESIAN_POINT('Ctrl Pts',(-74.2170326445434,44.5625000013656,-74.2170326445434));
#7865=CARTESIAN_POINT('Ctrl Pts',(-43.4753311640868,44.5000000013656,-104.958734125));
#7866=CARTESIAN_POINT('Ctrl Pts',(-6.42686888943697E-15,44.4375000013656,
-104.958734125));
#7867=CARTESIAN_POINT('Ctrl Pts',(43.4753311640868,44.3750000013656,-104.958734125));
#7868=CARTESIAN_POINT('Ctrl Pts',(74.2170326445434,44.3125000013656,-74.2170326445434));
#7869=CARTESIAN_POINT('Ctrl Pts',(104.958734125,44.2500000013656,-43.4753311640868));
#7870=CARTESIAN_POINT('Ctrl Pts',(104.958734125,44.1875000013656,-1.28537377788739E-14));
#7871=CARTESIAN_POINT('Ctrl Pts',(104.958734125,44.1250000013656,43.4753311640868));
#7872=CARTESIAN_POINT('Ctrl Pts',(74.2170326445434,44.0625000013656,74.2170326445434));
#7873=CARTESIAN_POINT('Ctrl Pts',(43.4753311640869,44.0000000013656,104.958734125));
#7874=CARTESIAN_POINT('Ctrl Pts',(1.92806066683109E-14,43.9375000013656,
104.958734125));
#7875=CARTESIAN_POINT('Ctrl Pts',(-43.4753311640868,43.8750000013656,104.958734125));
#7876=CARTESIAN_POINT('Ctrl Pts',(-74.2170326445434,43.8125000013656,74.2170326445434));
#7877=CARTESIAN_POINT('Ctrl Pts',(-104.958734125,43.7500000013656,43.4753311640869));
#7878=CARTESIAN_POINT('Ctrl Pts',(-104.958734125,43.6875000013656,0.));
#7879=CARTESIAN_POINT('Ctrl Pts',(-104.958734125,43.6250000013656,-43.4753311640868));
#7880=CARTESIAN_POINT('Ctrl Pts',(-74.2170326445434,43.5625000013656,-74.2170326445434));
#7881=CARTESIAN_POINT('Ctrl Pts',(-43.4753311640868,43.5000000013656,-104.958734125));
#7882=CARTESIAN_POINT('Ctrl Pts',(-6.42686888943697E-15,43.4375000013656,
-104.958734125));
#7883=CARTESIAN_POINT('Ctrl Pts',(43.4753311640868,43.3750000013656,-104.958734125));
#7884=CARTESIAN_POINT('Ctrl Pts',(74.2170326445434,43.3125000013656,-74.2170326445434));
#7885=CARTESIAN_POINT('Ctrl Pts',(104.958734125,43.2500000013656,-43.4753311640868));
#7886=CARTESIAN_POINT('Ctrl Pts',(104.958734125,43.1875000013656,-1.28537377788739E-14));
#7887=CARTESIAN_POINT('Ctrl Pts',(104.958734125,43.1250000013656,43.4753311640868));
#7888=CARTESIAN_POINT('Ctrl Pts',(74.2170326445434,43.0625000013656,74.2170326445434));
#7889=CARTESIAN_POINT('Ctrl Pts',(43.4753311640869,43.0000000013656,104.958734125));
#7890=CARTESIAN_POINT('Ctrl Pts',(1.92806066683109E-14,42.9375000013656,
104.958734125));
#7891=CARTESIAN_POINT('Ctrl Pts',(-43.4753311640868,42.8750000013656,104.958734125));
#7892=CARTESIAN_POINT('Ctrl Pts',(-74.2170326445434,42.8125000013656,74.2170326445434));
#7893=CARTESIAN_POINT('Ctrl Pts',(-104.958734125,42.7500000013656,43.4753311640869));
#7894=CARTESIAN_POINT('Ctrl Pts',(-104.958734125,42.6875000013656,0.));
#7895=CARTESIAN_POINT('Ctrl Pts',(-104.958734125,42.6250000013656,-43.4753311640868));
#7896=CARTESIAN_POINT('Ctrl Pts',(-74.2170326445434,42.5625000013656,-74.2170326445434));
#7897=CARTESIAN_POINT('Ctrl Pts',(-43.4753311640868,42.5000000013656,-104.958734125));
#7898=CARTESIAN_POINT('Ctrl Pts',(-6.42686888943697E-15,42.4375000013656,
-104.958734125));
#7899=CARTESIAN_POINT('Ctrl Pts',(43.4753311640868,42.3750000013656,-104.958734125));
#7900=CARTESIAN_POINT('Ctrl Pts',(74.2170326445434,42.3125000013656,-74.2170326445434));
#7901=CARTESIAN_POINT('Ctrl Pts',(104.958734125,42.2500000013656,-43.4753311640868));
#7902=CARTESIAN_POINT('Ctrl Pts',(104.958734125,42.1875000013656,-1.28537377788739E-14));
#7903=CARTESIAN_POINT('Ctrl Pts',(104.958734125,42.1250000013656,43.4753311640868));
#7904=CARTESIAN_POINT('Ctrl Pts',(74.2170326445434,42.0625000013656,74.2170326445434));
#7905=CARTESIAN_POINT('Ctrl Pts',(43.4753311640869,42.0000000013656,104.958734125));
#7906=CARTESIAN_POINT('Ctrl Pts',(1.92806066683109E-14,41.9375000013656,
104.958734125));
#7907=CARTESIAN_POINT('Ctrl Pts',(-43.4753311640868,41.8750000013656,104.958734125));
#7908=CARTESIAN_POINT('Ctrl Pts',(-74.2170326445434,41.8125000013656,74.2170326445434));
#7909=CARTESIAN_POINT('Ctrl Pts',(-104.958734125,41.7500000013656,43.4753311640869));
#7910=CARTESIAN_POINT('Ctrl Pts',(-104.958734125,41.6875000013656,0.));
#7911=CARTESIAN_POINT('Ctrl Pts',(-104.958734125,41.6250000013656,-43.4753311640868));
#7912=CARTESIAN_POINT('Ctrl Pts',(-74.2170326445434,41.5625000013656,-74.2170326445434));
#7913=CARTESIAN_POINT('Ctrl Pts',(-43.4753311640868,41.5000000013656,-104.958734125));
#7914=CARTESIAN_POINT('Ctrl Pts',(-6.42686888943697E-15,41.4375000013656,
-104.958734125));
#7915=CARTESIAN_POINT('Ctrl Pts',(43.4753311640868,41.3750000013656,-104.958734125));
#7916=CARTESIAN_POINT('Ctrl Pts',(74.2170326445434,41.3125000013656,-74.2170326445434));
#7917=CARTESIAN_POINT('Ctrl Pts',(104.958734125,41.2500000013656,-43.4753311640868));
#7918=CARTESIAN_POINT('Ctrl Pts',(104.958734125,41.1875000013656,-1.28537377788739E-14));
#7919=CARTESIAN_POINT('Ctrl Pts',(104.958734125,41.1250000013656,43.4753311640868));
#7920=CARTESIAN_POINT('Ctrl Pts',(74.2170326445434,41.0625000013656,74.2170326445434));
#7921=CARTESIAN_POINT('Ctrl Pts',(43.4753311640869,41.0000000013656,104.958734125));
#7922=CARTESIAN_POINT('Ctrl Pts',(1.92806066683109E-14,40.9375000013656,
104.958734125));
#7923=CARTESIAN_POINT('Ctrl Pts',(-43.4753311640868,40.8750000013656,104.958734125));
#7924=CARTESIAN_POINT('Ctrl Pts',(-74.2170326445434,40.8125000013656,74.2170326445434));
#7925=CARTESIAN_POINT('Ctrl Pts',(-104.958734125,40.7500000013656,43.4753311640869));
#7926=CARTESIAN_POINT('Ctrl Pts',(-104.958734125,40.6875000013656,0.));
#7927=CARTESIAN_POINT('Ctrl Pts',(-104.958734125,40.6250000013656,-43.4753311640868));
#7928=CARTESIAN_POINT('Ctrl Pts',(-74.2170326445434,40.5625000013656,-74.2170326445434));
#7929=CARTESIAN_POINT('Ctrl Pts',(-43.4753311640868,40.5000000013656,-104.958734125));
#7930=CARTESIAN_POINT('Ctrl Pts',(-6.42686888943697E-15,40.4375000013656,
-104.958734125));
#7931=CARTESIAN_POINT('Ctrl Pts',(43.4753311640868,40.3750000013656,-104.958734125));
#7932=CARTESIAN_POINT('Ctrl Pts',(74.2170326445434,40.3125000013656,-74.2170326445434));
#7933=CARTESIAN_POINT('Ctrl Pts',(104.958734125,40.2500000013656,-43.4753311640868));
#7934=CARTESIAN_POINT('Ctrl Pts',(104.958734125,40.1875000013656,-1.28537377788739E-14));
#7935=CARTESIAN_POINT('Ctrl Pts',(104.958734125,40.1250000013656,43.4753311640868));
#7936=CARTESIAN_POINT('Ctrl Pts',(74.2170326445434,40.0625000013656,74.2170326445434));
#7937=CARTESIAN_POINT('Ctrl Pts',(43.4753311640869,40.0000000013656,104.958734125));
#7938=CARTESIAN_POINT('Ctrl Pts',(1.92806066683109E-14,39.9375000013656,
104.958734125));
#7939=CARTESIAN_POINT('Ctrl Pts',(-43.4753311640868,39.8750000013656,104.958734125));
#7940=CARTESIAN_POINT('Ctrl Pts',(-74.2170326445434,39.8125000013656,74.2170326445434));
#7941=CARTESIAN_POINT('Ctrl Pts',(-104.958734125,39.7500000013656,43.4753311640869));
#7942=CARTESIAN_POINT('Ctrl Pts',(-104.958734125,39.6875000013656,0.));
#7943=CARTESIAN_POINT('Ctrl Pts',(-104.958734125,39.6250000013656,-43.4753311640868));
#7944=CARTESIAN_POINT('Ctrl Pts',(-74.2170326445434,39.5625000013656,-74.2170326445434));
#7945=CARTESIAN_POINT('Ctrl Pts',(-43.4753311640868,39.5000000013656,-104.958734125));
#7946=CARTESIAN_POINT('Ctrl Pts',(-6.42686888943697E-15,39.4375000013656,
-104.958734125));
#7947=CARTESIAN_POINT('Ctrl Pts',(43.4753311640868,39.3750000013656,-104.958734125));
#7948=CARTESIAN_POINT('Ctrl Pts',(74.2170326445434,39.3125000013656,-74.2170326445434));
#7949=CARTESIAN_POINT('Ctrl Pts',(104.958734125,39.2500000013656,-43.4753311640868));
#7950=CARTESIAN_POINT('Ctrl Pts',(104.958734125,39.1875000013656,-1.28537377788739E-14));
#7951=CARTESIAN_POINT('Ctrl Pts',(104.958734125,39.1250000013656,43.4753311640868));
#7952=CARTESIAN_POINT('Ctrl Pts',(74.2170326445434,39.0625000013656,74.2170326445434));
#7953=CARTESIAN_POINT('Ctrl Pts',(43.4753311640869,39.0000000013656,104.958734125));
#7954=CARTESIAN_POINT('Ctrl Pts',(1.92806066683109E-14,38.9375000013656,
104.958734125));
#7955=CARTESIAN_POINT('Ctrl Pts',(-43.4753311640868,38.8750000013656,104.958734125));
#7956=CARTESIAN_POINT('Ctrl Pts',(-74.2170326445434,38.8125000013656,74.2170326445434));
#7957=CARTESIAN_POINT('Ctrl Pts',(-104.958734125,38.7500000013656,43.4753311640869));
#7958=CARTESIAN_POINT('Ctrl Pts',(-104.958734125,38.6875000013656,0.));
#7959=CARTESIAN_POINT('Ctrl Pts',(-104.958734125,38.6250000013656,-43.4753311640868));
#7960=CARTESIAN_POINT('Ctrl Pts',(-74.2170326445434,38.5625000013656,-74.2170326445434));
#7961=CARTESIAN_POINT('Ctrl Pts',(-43.4753311640868,38.5000000013656,-104.958734125));
#7962=CARTESIAN_POINT('Ctrl Pts',(-6.42686888943697E-15,38.4375000013656,
-104.958734125));
#7963=CARTESIAN_POINT('Ctrl Pts',(43.4753311640868,38.3750000013656,-104.958734125));
#7964=CARTESIAN_POINT('Ctrl Pts',(74.2170326445434,38.3125000013656,-74.2170326445434));
#7965=CARTESIAN_POINT('Ctrl Pts',(104.958734125,38.2500000013656,-43.4753311640868));
#7966=CARTESIAN_POINT('Ctrl Pts',(104.958734125,38.1875000013656,-1.28537377788739E-14));
#7967=CARTESIAN_POINT('Ctrl Pts',(104.958734125,38.1250000013656,43.4753311640868));
#7968=CARTESIAN_POINT('Ctrl Pts',(74.2170326445434,38.0625000013656,74.2170326445434));
#7969=CARTESIAN_POINT('Ctrl Pts',(43.4753311640869,38.0000000013656,104.958734125));
#7970=CARTESIAN_POINT('Ctrl Pts',(1.92806066683109E-14,37.9375000013656,
104.958734125));
#7971=CARTESIAN_POINT('Ctrl Pts',(-43.4753311640868,37.8750000013656,104.958734125));
#7972=CARTESIAN_POINT('Ctrl Pts',(-74.2170326445434,37.8125000013656,74.2170326445434));
#7973=CARTESIAN_POINT('Ctrl Pts',(-104.958734125,37.7500000013656,43.4753311640869));
#7974=CARTESIAN_POINT('Ctrl Pts',(-104.958734125,37.6875000013656,0.));
#7975=CARTESIAN_POINT('Ctrl Pts',(-104.958734125,37.6250000013656,-43.4753311640868));
#7976=CARTESIAN_POINT('Ctrl Pts',(-74.2170326445434,37.5625000013656,-74.2170326445434));
#7977=CARTESIAN_POINT('Ctrl Pts',(-43.4753311640868,37.5000000013656,-104.958734125));
#7978=CARTESIAN_POINT('Ctrl Pts',(-6.42686888943697E-15,37.4375000013656,
-104.958734125));
#7979=CARTESIAN_POINT('Ctrl Pts',(43.4753311640868,37.3750000013656,-104.958734125));
#7980=CARTESIAN_POINT('Ctrl Pts',(74.2170326445434,37.3125000013656,-74.2170326445434));
#7981=CARTESIAN_POINT('Ctrl Pts',(104.958734125,37.2500000013656,-43.4753311640868));
#7982=CARTESIAN_POINT('Ctrl Pts',(104.958734125,37.1875000013656,-1.28537377788739E-14));
#7983=CARTESIAN_POINT('Ctrl Pts',(104.958734125,37.1250000013656,43.4753311640868));
#7984=CARTESIAN_POINT('Ctrl Pts',(74.2170326445434,37.0625000013656,74.2170326445434));
#7985=CARTESIAN_POINT('Ctrl Pts',(43.4753311640869,37.0000000013656,104.958734125));
#7986=CARTESIAN_POINT('Ctrl Pts',(1.92806066683109E-14,36.9375000013656,
104.958734125));
#7987=CARTESIAN_POINT('Ctrl Pts',(-43.4753311640868,36.8750000013656,104.958734125));
#7988=CARTESIAN_POINT('Ctrl Pts',(-74.2170326445434,36.8125000013656,74.2170326445434));
#7989=CARTESIAN_POINT('Ctrl Pts',(-104.958734125,36.7500000013656,43.4753311640869));
#7990=CARTESIAN_POINT('Ctrl Pts',(-104.958734125,36.6875000013656,0.));
#7991=CARTESIAN_POINT('Ctrl Pts',(-104.958734125,36.6250000013656,-43.4753311640868));
#7992=CARTESIAN_POINT('Ctrl Pts',(-74.2170326445434,36.5625000013656,-74.2170326445434));
#7993=CARTESIAN_POINT('Ctrl Pts',(-43.4753311640868,36.5000000013656,-104.958734125));
#7994=CARTESIAN_POINT('Ctrl Pts',(-6.42686888943697E-15,36.4375000013656,
-104.958734125));
#7995=CARTESIAN_POINT('Ctrl Pts',(43.4753311640868,36.3750000013656,-104.958734125));
#7996=CARTESIAN_POINT('Ctrl Pts',(74.2170326445434,36.3125000013656,-74.2170326445434));
#7997=CARTESIAN_POINT('Ctrl Pts',(104.958734125,36.2500000013656,-43.4753311640868));
#7998=CARTESIAN_POINT('Ctrl Pts',(104.958734125,36.1875000013656,-1.28537377788739E-14));
#7999=CARTESIAN_POINT('Ctrl Pts',(104.958734125,36.1250000013656,43.4753311640868));
#8000=CARTESIAN_POINT('Ctrl Pts',(74.2170326445434,36.0625000013656,74.2170326445434));
#8001=CARTESIAN_POINT('Ctrl Pts',(43.4753311640869,36.0000000013656,104.958734125));
#8002=CARTESIAN_POINT('Ctrl Pts',(1.92806066683109E-14,35.9375000013656,
104.958734125));
#8003=CARTESIAN_POINT('Ctrl Pts',(-43.4753311640868,35.8750000013656,104.958734125));
#8004=CARTESIAN_POINT('Ctrl Pts',(-74.2170326445434,35.8125000013656,74.2170326445434));
#8005=CARTESIAN_POINT('Ctrl Pts',(-104.958734125,35.7500000013656,43.4753311640869));
#8006=CARTESIAN_POINT('Ctrl Pts',(-104.958734125,35.6875000013656,0.));
#8007=CARTESIAN_POINT('Ctrl Pts',(-104.958734125,35.6250000013656,-43.4753311640868));
#8008=CARTESIAN_POINT('Ctrl Pts',(-74.2170326445434,35.5625000013656,-74.2170326445434));
#8009=CARTESIAN_POINT('Ctrl Pts',(-43.4753311640868,35.5000000013656,-104.958734125));
#8010=CARTESIAN_POINT('Ctrl Pts',(-6.42686888943697E-15,35.4375000013656,
-104.958734125));
#8011=CARTESIAN_POINT('Ctrl Pts',(43.4753311640868,35.3750000013656,-104.958734125));
#8012=CARTESIAN_POINT('Ctrl Pts',(74.2170326445434,35.3125000013656,-74.2170326445434));
#8013=CARTESIAN_POINT('Ctrl Pts',(104.958734125,35.2500000013656,-43.4753311640868));
#8014=CARTESIAN_POINT('Ctrl Pts',(104.958734125,35.1875000013656,-1.28537377788739E-14));
#8015=CARTESIAN_POINT('Ctrl Pts',(104.958734125,35.1250000013656,43.4753311640868));
#8016=CARTESIAN_POINT('Ctrl Pts',(74.2170326445434,35.0625000013656,74.2170326445434));
#8017=CARTESIAN_POINT('Ctrl Pts',(43.4753311640869,35.0000000013656,104.958734125));
#8018=CARTESIAN_POINT('Ctrl Pts',(1.92806066683109E-14,34.9375000013656,
104.958734125));
#8019=CARTESIAN_POINT('Ctrl Pts',(-43.4753311640868,34.8750000013656,104.958734125));
#8020=CARTESIAN_POINT('Ctrl Pts',(-74.2170326445434,34.8125000013656,74.2170326445434));
#8021=CARTESIAN_POINT('Ctrl Pts',(-104.958734125,34.7500000013656,43.4753311640869));
#8022=CARTESIAN_POINT('Ctrl Pts',(-104.958734125,34.6875000013656,0.));
#8023=CARTESIAN_POINT('Ctrl Pts',(-104.958734125,34.6250000013656,-43.4753311640868));
#8024=CARTESIAN_POINT('Ctrl Pts',(-74.2170326445434,34.5625000013656,-74.2170326445434));
#8025=CARTESIAN_POINT('Ctrl Pts',(-43.4753311640868,34.5000000013656,-104.958734125));
#8026=CARTESIAN_POINT('Ctrl Pts',(-6.42686888943697E-15,34.4375000013656,
-104.958734125));
#8027=CARTESIAN_POINT('Ctrl Pts',(43.4753311640868,34.3750000013656,-104.958734125));
#8028=CARTESIAN_POINT('Ctrl Pts',(74.2170326445434,34.3125000013656,-74.2170326445434));
#8029=CARTESIAN_POINT('Ctrl Pts',(104.958734125,34.2500000013656,-43.4753311640868));
#8030=CARTESIAN_POINT('Ctrl Pts',(104.958734125,34.1875000013656,-1.28537377788739E-14));
#8031=CARTESIAN_POINT('Ctrl Pts',(104.958734125,34.1250000013656,43.4753311640868));
#8032=CARTESIAN_POINT('Ctrl Pts',(74.2170326445434,34.0625000013656,74.2170326445434));
#8033=CARTESIAN_POINT('Ctrl Pts',(43.4753311640869,34.0000000013656,104.958734125));
#8034=CARTESIAN_POINT('Ctrl Pts',(1.92806066683109E-14,33.9375000013656,
104.958734125));
#8035=CARTESIAN_POINT('Ctrl Pts',(-43.4753311640868,33.8750000013656,104.958734125));
#8036=CARTESIAN_POINT('Ctrl Pts',(-74.2170326445434,33.8125000013656,74.2170326445434));
#8037=CARTESIAN_POINT('Ctrl Pts',(-104.958734125,33.7500000013656,43.4753311640869));
#8038=CARTESIAN_POINT('Ctrl Pts',(-104.958734125,33.6875000013656,0.));
#8039=CARTESIAN_POINT('Ctrl Pts',(-104.958734125,33.6250000013656,-43.4753311640868));
#8040=CARTESIAN_POINT('Ctrl Pts',(-74.2170326445434,33.5625000013656,-74.2170326445434));
#8041=CARTESIAN_POINT('Ctrl Pts',(-43.4753311640868,33.5000000013656,-104.958734125));
#8042=CARTESIAN_POINT('Ctrl Pts',(-6.42686888943697E-15,33.4375000013656,
-104.958734125));
#8043=CARTESIAN_POINT('Ctrl Pts',(43.4753311640868,33.3750000013656,-104.958734125));
#8044=CARTESIAN_POINT('Ctrl Pts',(74.2170326445434,33.3125000013656,-74.2170326445434));
#8045=CARTESIAN_POINT('Ctrl Pts',(104.958734125,33.2500000013656,-43.4753311640868));
#8046=CARTESIAN_POINT('Ctrl Pts',(104.958734125,33.1875000013656,-1.28537377788739E-14));
#8047=CARTESIAN_POINT('Ctrl Pts',(104.958734125,33.1250000013656,43.4753311640868));
#8048=CARTESIAN_POINT('Ctrl Pts',(74.2170326445434,33.0625000013656,74.2170326445434));
#8049=CARTESIAN_POINT('Ctrl Pts',(43.4753311640869,33.0000000013656,104.958734125));
#8050=CARTESIAN_POINT('Ctrl Pts',(1.92806066683109E-14,32.9375000013656,
104.958734125));
#8051=CARTESIAN_POINT('Ctrl Pts',(-43.4753311640868,32.8750000013656,104.958734125));
#8052=CARTESIAN_POINT('Ctrl Pts',(-74.2170326445434,32.8125000013656,74.2170326445434));
#8053=CARTESIAN_POINT('Ctrl Pts',(-104.958734125,32.7500000013656,43.4753311640869));
#8054=CARTESIAN_POINT('Ctrl Pts',(-104.958734125,32.6875000013656,0.));
#8055=CARTESIAN_POINT('Ctrl Pts',(-104.958734125,32.6250000013656,-43.4753311640868));
#8056=CARTESIAN_POINT('Ctrl Pts',(-74.2170326445434,32.5625000013656,-74.2170326445434));
#8057=CARTESIAN_POINT('Ctrl Pts',(-43.4753311640868,32.5000000013656,-104.958734125));
#8058=CARTESIAN_POINT('Ctrl Pts',(-6.42686888943697E-15,32.4375000013656,
-104.958734125));
#8059=CARTESIAN_POINT('Ctrl Pts',(43.4753311640868,32.3750000013656,-104.958734125));
#8060=CARTESIAN_POINT('Ctrl Pts',(74.2170326445434,32.3125000013656,-74.2170326445434));
#8061=CARTESIAN_POINT('Ctrl Pts',(104.958734125,32.2500000013656,-43.4753311640868));
#8062=CARTESIAN_POINT('Ctrl Pts',(104.958734125,32.1875000013656,-1.28537377788739E-14));
#8063=CARTESIAN_POINT('Ctrl Pts',(104.958734125,32.1250000013656,43.4753311640868));
#8064=CARTESIAN_POINT('Ctrl Pts',(74.2170326445434,32.0625000013656,74.2170326445434));
#8065=CARTESIAN_POINT('Ctrl Pts',(43.4753311640869,32.0000000013656,104.958734125));
#8066=CARTESIAN_POINT('Ctrl Pts',(1.92806066683109E-14,31.9375000013656,
104.958734125));
#8067=CARTESIAN_POINT('Ctrl Pts',(-43.4753311640868,31.8750000013656,104.958734125));
#8068=CARTESIAN_POINT('Ctrl Pts',(-74.2170326445434,31.8125000013656,74.2170326445434));
#8069=CARTESIAN_POINT('Ctrl Pts',(-104.958734125,31.7500000013656,43.4753311640869));
#8070=CARTESIAN_POINT('Ctrl Pts',(-104.958734125,31.6875000013656,0.));
#8071=CARTESIAN_POINT('Ctrl Pts',(-104.958734125,31.6250000013656,-43.4753311640868));
#8072=CARTESIAN_POINT('Ctrl Pts',(-74.2170326445434,31.5625000013656,-74.2170326445434));
#8073=CARTESIAN_POINT('Ctrl Pts',(-43.4753311640868,31.5000000013656,-104.958734125));
#8074=CARTESIAN_POINT('Ctrl Pts',(-6.42686888943697E-15,31.4375000013656,
-104.958734125));
#8075=CARTESIAN_POINT('Ctrl Pts',(43.4753311640868,31.3750000013656,-104.958734125));
#8076=CARTESIAN_POINT('Ctrl Pts',(74.2170326445434,31.3125000013656,-74.2170326445434));
#8077=CARTESIAN_POINT('Ctrl Pts',(104.958734125,31.2500000013656,-43.4753311640868));
#8078=CARTESIAN_POINT('Ctrl Pts',(104.958734125,31.1875000013656,-1.28537377788739E-14));
#8079=CARTESIAN_POINT('Ctrl Pts',(104.958734125,31.1250000013656,43.4753311640868));
#8080=CARTESIAN_POINT('Ctrl Pts',(74.2170326445434,31.0625000013656,74.2170326445434));
#8081=CARTESIAN_POINT('Ctrl Pts',(43.4753311640869,31.0000000013656,104.958734125));
#8082=CARTESIAN_POINT('Ctrl Pts',(1.92806066683109E-14,30.9375000013656,
104.958734125));
#8083=CARTESIAN_POINT('Ctrl Pts',(-43.4753311640868,30.8750000013656,104.958734125));
#8084=CARTESIAN_POINT('Ctrl Pts',(-74.2170326445434,30.8125000013656,74.2170326445434));
#8085=CARTESIAN_POINT('Ctrl Pts',(-104.958734125,30.7500000013656,43.4753311640869));
#8086=CARTESIAN_POINT('Ctrl Pts',(-104.958734125,30.6875000013656,0.));
#8087=CARTESIAN_POINT('Ctrl Pts',(-104.958734125,30.6250000013656,-43.4753311640868));
#8088=CARTESIAN_POINT('Ctrl Pts',(-74.2170326445434,30.5625000013656,-74.2170326445434));
#8089=CARTESIAN_POINT('Ctrl Pts',(-43.4753311640868,30.5000000013656,-104.958734125));
#8090=CARTESIAN_POINT('Ctrl Pts',(-6.42686888943697E-15,30.4375000013656,
-104.958734125));
#8091=CARTESIAN_POINT('Ctrl Pts',(43.4753311640868,30.3750000013656,-104.958734125));
#8092=CARTESIAN_POINT('Ctrl Pts',(74.2170326445434,30.3125000013656,-74.2170326445434));
#8093=CARTESIAN_POINT('Ctrl Pts',(104.958734125,30.2500000013656,-43.4753311640868));
#8094=CARTESIAN_POINT('Ctrl Pts',(104.958734125,30.1875000013656,-1.28537377788739E-14));
#8095=CARTESIAN_POINT('Ctrl Pts',(104.958734125,30.1250000013656,43.4753311640868));
#8096=CARTESIAN_POINT('Ctrl Pts',(74.2170326445434,30.0625000013656,74.2170326445434));
#8097=CARTESIAN_POINT('Ctrl Pts',(43.4753311640869,30.0000000013656,104.958734125));
#8098=CARTESIAN_POINT('Ctrl Pts',(1.92806066683109E-14,29.9375000013656,
104.958734125));
#8099=CARTESIAN_POINT('Ctrl Pts',(-43.4753311640868,29.8750000013656,104.958734125));
#8100=CARTESIAN_POINT('Ctrl Pts',(-74.2170326445434,29.8125000013656,74.2170326445434));
#8101=CARTESIAN_POINT('Ctrl Pts',(-104.958734125,29.7500000013656,43.4753311640869));
#8102=CARTESIAN_POINT('Ctrl Pts',(-104.958734125,29.6875000013656,0.));
#8103=CARTESIAN_POINT('Ctrl Pts',(-104.958734125,29.6250000013656,-43.4753311640868));
#8104=CARTESIAN_POINT('Ctrl Pts',(-74.2170326445434,29.5625000013656,-74.2170326445434));
#8105=CARTESIAN_POINT('Ctrl Pts',(-43.4753311640868,29.5000000013656,-104.958734125));
#8106=CARTESIAN_POINT('Ctrl Pts',(-6.42686888943697E-15,29.4375000013656,
-104.958734125));
#8107=CARTESIAN_POINT('Ctrl Pts',(43.4753311640868,29.3750000013656,-104.958734125));
#8108=CARTESIAN_POINT('Ctrl Pts',(74.2170326445434,29.3125000013656,-74.2170326445434));
#8109=CARTESIAN_POINT('Ctrl Pts',(104.958734125,29.2500000013656,-43.4753311640868));
#8110=CARTESIAN_POINT('Ctrl Pts',(104.958734125,29.1875000013656,-1.28537377788739E-14));
#8111=CARTESIAN_POINT('Ctrl Pts',(104.958734125,29.1250000013656,43.4753311640868));
#8112=CARTESIAN_POINT('Ctrl Pts',(74.2170326445434,29.0625000013656,74.2170326445434));
#8113=CARTESIAN_POINT('Ctrl Pts',(43.4753311640869,29.0000000013656,104.958734125));
#8114=CARTESIAN_POINT('Ctrl Pts',(1.92806066683109E-14,28.9375000013656,
104.958734125));
#8115=CARTESIAN_POINT('Ctrl Pts',(-43.4753311640868,28.8750000013656,104.958734125));
#8116=CARTESIAN_POINT('Ctrl Pts',(-74.2170326445434,28.8125000013656,74.2170326445434));
#8117=CARTESIAN_POINT('Ctrl Pts',(-104.958734125,28.7500000013656,43.4753311640869));
#8118=CARTESIAN_POINT('Ctrl Pts',(-104.958734125,28.6875000013656,0.));
#8119=CARTESIAN_POINT('Ctrl Pts',(-104.958734125,28.6250000013656,-43.4753311640868));
#8120=CARTESIAN_POINT('Ctrl Pts',(-74.2170326445434,28.5625000013656,-74.2170326445434));
#8121=CARTESIAN_POINT('Ctrl Pts',(-43.4753311640868,28.5000000013656,-104.958734125));
#8122=CARTESIAN_POINT('Ctrl Pts',(-6.42686888943697E-15,28.4375000013656,
-104.958734125));
#8123=CARTESIAN_POINT('Ctrl Pts',(43.4753311640868,28.3750000013656,-104.958734125));
#8124=CARTESIAN_POINT('Ctrl Pts',(74.2170326445434,28.3125000013656,-74.2170326445434));
#8125=CARTESIAN_POINT('Ctrl Pts',(104.958734125,28.2500000013656,-43.4753311640868));
#8126=CARTESIAN_POINT('Ctrl Pts',(104.958734125,28.1875000013656,-1.28537377788739E-14));
#8127=CARTESIAN_POINT('Ctrl Pts',(104.958734125,28.1250000013656,43.4753311640868));
#8128=CARTESIAN_POINT('Ctrl Pts',(74.2170326445434,28.0625000013656,74.2170326445434));
#8129=CARTESIAN_POINT('Ctrl Pts',(43.4753311640869,28.0000000013656,104.958734125));
#8130=CARTESIAN_POINT('Ctrl Pts',(1.92806066683109E-14,27.9375000013656,
104.958734125));
#8131=CARTESIAN_POINT('Ctrl Pts',(-43.4753311640868,27.8750000013656,104.958734125));
#8132=CARTESIAN_POINT('Ctrl Pts',(-74.2170326445434,27.8125000013656,74.2170326445434));
#8133=CARTESIAN_POINT('Ctrl Pts',(-104.958734125,27.7500000013656,43.4753311640869));
#8134=CARTESIAN_POINT('Ctrl Pts',(-104.958734125,27.6875000013656,0.));
#8135=CARTESIAN_POINT('Ctrl Pts',(-104.958734125,27.6250000013656,-43.4753311640868));
#8136=CARTESIAN_POINT('Ctrl Pts',(-74.2170326445434,27.5625000013656,-74.2170326445434));
#8137=CARTESIAN_POINT('Ctrl Pts',(-43.4753311640868,27.5000000013656,-104.958734125));
#8138=CARTESIAN_POINT('Ctrl Pts',(-6.42686888943697E-15,27.4375000013656,
-104.958734125));
#8139=CARTESIAN_POINT('Ctrl Pts',(43.4753311640868,27.3750000013656,-104.958734125));
#8140=CARTESIAN_POINT('Ctrl Pts',(74.2170326445434,27.3125000013656,-74.2170326445434));
#8141=CARTESIAN_POINT('Ctrl Pts',(104.958734125,27.2500000013656,-43.4753311640868));
#8142=CARTESIAN_POINT('Ctrl Pts',(104.958734125,27.1875000013656,-1.28537377788739E-14));
#8143=CARTESIAN_POINT('Ctrl Pts',(104.958734125,27.1250000013656,43.4753311640868));
#8144=CARTESIAN_POINT('Ctrl Pts',(74.2170326445434,27.0625000013656,74.2170326445434));
#8145=CARTESIAN_POINT('Ctrl Pts',(43.4753311640869,27.0000000013656,104.958734125));
#8146=CARTESIAN_POINT('Ctrl Pts',(1.92806066683109E-14,26.9375000013656,
104.958734125));
#8147=CARTESIAN_POINT('Ctrl Pts',(-43.4753311640868,26.8750000013656,104.958734125));
#8148=CARTESIAN_POINT('Ctrl Pts',(-74.2170326445434,26.8125000013656,74.2170326445434));
#8149=CARTESIAN_POINT('Ctrl Pts',(-104.958734125,26.7500000013656,43.4753311640869));
#8150=CARTESIAN_POINT('Ctrl Pts',(-104.958734125,26.6875000013656,0.));
#8151=CARTESIAN_POINT('Ctrl Pts',(-104.958734125,26.6250000013656,-43.4753311640868));
#8152=CARTESIAN_POINT('Ctrl Pts',(-74.2170326445434,26.5625000013656,-74.2170326445434));
#8153=CARTESIAN_POINT('Ctrl Pts',(-43.4753311640868,26.5000000013656,-104.958734125));
#8154=CARTESIAN_POINT('Ctrl Pts',(-6.42686888943697E-15,26.4375000013656,
-104.958734125));
#8155=CARTESIAN_POINT('Ctrl Pts',(43.4753311640868,26.3750000013656,-104.958734125));
#8156=CARTESIAN_POINT('Ctrl Pts',(74.2170326445434,26.3125000013656,-74.2170326445434));
#8157=CARTESIAN_POINT('Ctrl Pts',(104.958734125,26.2500000013656,-43.4753311640868));
#8158=CARTESIAN_POINT('Ctrl Pts',(104.958734125,26.1875000013656,-1.28537377788739E-14));
#8159=CARTESIAN_POINT('Ctrl Pts',(104.958734125,26.1250000013656,43.4753311640868));
#8160=CARTESIAN_POINT('Ctrl Pts',(74.2170326445434,26.0625000013656,74.2170326445434));
#8161=CARTESIAN_POINT('Ctrl Pts',(43.4753311640869,26.0000000013656,104.958734125));
#8162=CARTESIAN_POINT('Ctrl Pts',(1.92806066683109E-14,25.9375000013656,
104.958734125));
#8163=CARTESIAN_POINT('Ctrl Pts',(-43.4753311640868,25.8750000013656,104.958734125));
#8164=CARTESIAN_POINT('Ctrl Pts',(-74.2170326445434,25.8125000013656,74.2170326445434));
#8165=CARTESIAN_POINT('Ctrl Pts',(-104.958734125,25.7500000013656,43.4753311640869));
#8166=CARTESIAN_POINT('Ctrl Pts',(-104.958734125,25.6875000013656,0.));
#8167=CARTESIAN_POINT('Ctrl Pts',(-104.958734125,25.6250000013656,-43.4753311640868));
#8168=CARTESIAN_POINT('Ctrl Pts',(-74.2170326445434,25.5625000013656,-74.2170326445434));
#8169=CARTESIAN_POINT('Ctrl Pts',(-43.4753311640868,25.5000000013656,-104.958734125));
#8170=CARTESIAN_POINT('Ctrl Pts',(-6.42686888943697E-15,25.4375000013656,
-104.958734125));
#8171=CARTESIAN_POINT('Ctrl Pts',(43.4753311640868,25.3750000013656,-104.958734125));
#8172=CARTESIAN_POINT('Ctrl Pts',(74.2170326445434,25.3125000013656,-74.2170326445434));
#8173=CARTESIAN_POINT('Ctrl Pts',(104.958734125,25.2500000013656,-43.4753311640868));
#8174=CARTESIAN_POINT('Ctrl Pts',(104.958734125,25.1875000013656,-1.28537377788739E-14));
#8175=CARTESIAN_POINT('Ctrl Pts',(104.958734125,25.1250000013656,43.4753311640868));
#8176=CARTESIAN_POINT('Ctrl Pts',(74.2170326445434,25.0625000013656,74.2170326445434));
#8177=CARTESIAN_POINT('Ctrl Pts',(43.4753311640869,25.0000000013656,104.958734125));
#8178=CARTESIAN_POINT('Ctrl Pts',(1.92806066683109E-14,24.9375000013656,
104.958734125));
#8179=CARTESIAN_POINT('Ctrl Pts',(-43.4753311640868,24.8750000013656,104.958734125));
#8180=CARTESIAN_POINT('Ctrl Pts',(-74.2170326445434,24.8125000013656,74.2170326445434));
#8181=CARTESIAN_POINT('Ctrl Pts',(-104.958734125,24.7500000013656,43.4753311640869));
#8182=CARTESIAN_POINT('Ctrl Pts',(-104.958734125,24.6875000013656,0.));
#8183=CARTESIAN_POINT('Ctrl Pts',(-104.958734125,24.6250000013656,-43.4753311640868));
#8184=CARTESIAN_POINT('Ctrl Pts',(-74.2170326445434,24.5625000013656,-74.2170326445434));
#8185=CARTESIAN_POINT('Ctrl Pts',(-43.4753311640868,24.5000000013656,-104.958734125));
#8186=CARTESIAN_POINT('Ctrl Pts',(-6.42686888943697E-15,24.4375000013656,
-104.958734125));
#8187=CARTESIAN_POINT('Ctrl Pts',(43.4753311640868,24.3750000013656,-104.958734125));
#8188=CARTESIAN_POINT('Ctrl Pts',(74.2170326445434,24.3125000013656,-74.2170326445434));
#8189=CARTESIAN_POINT('Ctrl Pts',(104.958734125,24.2500000013656,-43.4753311640868));
#8190=CARTESIAN_POINT('Ctrl Pts',(104.958734125,24.1875000013656,-1.28537377788739E-14));
#8191=CARTESIAN_POINT('Ctrl Pts',(104.958734125,24.1250000013656,43.4753311640868));
#8192=CARTESIAN_POINT('Ctrl Pts',(74.2170326445434,24.0625000013656,74.2170326445434));
#8193=CARTESIAN_POINT('Ctrl Pts',(43.4753311640869,24.0000000013656,104.958734125));
#8194=CARTESIAN_POINT('Ctrl Pts',(1.92806066683109E-14,23.9375000013656,
104.958734125));
#8195=CARTESIAN_POINT('Ctrl Pts',(-43.4753311640868,23.8750000013656,104.958734125));
#8196=CARTESIAN_POINT('Ctrl Pts',(-74.2170326445434,23.8125000013656,74.2170326445434));
#8197=CARTESIAN_POINT('Ctrl Pts',(-104.958734125,23.7500000013656,43.4753311640869));
#8198=CARTESIAN_POINT('Ctrl Pts',(-104.958734125,23.6875000013656,0.));
#8199=CARTESIAN_POINT('Ctrl Pts',(-104.958734125,23.6250000013656,-43.4753311640868));
#8200=CARTESIAN_POINT('Ctrl Pts',(-74.2170326445434,23.5625000013656,-74.2170326445434));
#8201=CARTESIAN_POINT('Ctrl Pts',(-43.4753311640868,23.5000000013656,-104.958734125));
#8202=CARTESIAN_POINT('Ctrl Pts',(-6.42686888943697E-15,23.4375000013656,
-104.958734125));
#8203=CARTESIAN_POINT('Ctrl Pts',(43.4753311640868,23.3750000013656,-104.958734125));
#8204=CARTESIAN_POINT('Ctrl Pts',(74.2170326445434,23.3125000013656,-74.2170326445434));
#8205=CARTESIAN_POINT('Ctrl Pts',(104.958734125,23.2500000013656,-43.4753311640868));
#8206=CARTESIAN_POINT('Ctrl Pts',(104.958734125,23.1875000013656,-1.28537377788739E-14));
#8207=CARTESIAN_POINT('Ctrl Pts',(104.958734125,23.1250000013656,43.4753311640868));
#8208=CARTESIAN_POINT('Ctrl Pts',(74.2170326445434,23.0625000013656,74.2170326445434));
#8209=CARTESIAN_POINT('Ctrl Pts',(43.4753311640869,23.0000000013656,104.958734125));
#8210=CARTESIAN_POINT('Ctrl Pts',(1.92806066683109E-14,22.9375000013656,
104.958734125));
#8211=CARTESIAN_POINT('Ctrl Pts',(-43.4753311640868,22.8750000013656,104.958734125));
#8212=CARTESIAN_POINT('Ctrl Pts',(-74.2170326445434,22.8125000013656,74.2170326445434));
#8213=CARTESIAN_POINT('Ctrl Pts',(-104.958734125,22.7500000013656,43.4753311640869));
#8214=CARTESIAN_POINT('Ctrl Pts',(-104.958734125,22.6875000013656,0.));
#8215=CARTESIAN_POINT('Ctrl Pts',(-104.958734125,22.6250000013656,-43.4753311640868));
#8216=CARTESIAN_POINT('Ctrl Pts',(-74.2170326445434,22.5625000013656,-74.2170326445434));
#8217=CARTESIAN_POINT('Ctrl Pts',(-43.4753311640868,22.5000000013656,-104.958734125));
#8218=CARTESIAN_POINT('Ctrl Pts',(-6.42686888943697E-15,22.4375000013656,
-104.958734125));
#8219=CARTESIAN_POINT('Ctrl Pts',(43.4753311640868,22.3750000013656,-104.958734125));
#8220=CARTESIAN_POINT('Ctrl Pts',(74.2170326445434,22.3125000013656,-74.2170326445434));
#8221=CARTESIAN_POINT('Ctrl Pts',(104.958734125,22.2500000013656,-43.4753311640868));
#8222=CARTESIAN_POINT('Ctrl Pts',(104.958734125,22.1875000013656,-1.28537377788739E-14));
#8223=CARTESIAN_POINT('Ctrl Pts',(104.958734125,22.1250000013656,43.4753311640868));
#8224=CARTESIAN_POINT('Ctrl Pts',(74.2170326445434,22.0625000013656,74.2170326445434));
#8225=CARTESIAN_POINT('Ctrl Pts',(43.4753311640869,22.0000000013656,104.958734125));
#8226=CARTESIAN_POINT('Ctrl Pts',(1.92806066683109E-14,21.9375000013656,
104.958734125));
#8227=CARTESIAN_POINT('Ctrl Pts',(-43.4753311640868,21.8750000013656,104.958734125));
#8228=CARTESIAN_POINT('Ctrl Pts',(-74.2170326445434,21.8125000013656,74.2170326445434));
#8229=CARTESIAN_POINT('Ctrl Pts',(-104.958734125,21.7500000013656,43.4753311640869));
#8230=CARTESIAN_POINT('Ctrl Pts',(-104.958734125,21.6875000013656,0.));
#8231=CARTESIAN_POINT('Ctrl Pts',(-104.958734125,21.6250000013656,-43.4753311640868));
#8232=CARTESIAN_POINT('Ctrl Pts',(-74.2170326445434,21.5625000013656,-74.2170326445434));
#8233=CARTESIAN_POINT('Ctrl Pts',(-43.4753311640868,21.5000000013656,-104.958734125));
#8234=CARTESIAN_POINT('Ctrl Pts',(-6.42686888943697E-15,21.4375000013656,
-104.958734125));
#8235=CARTESIAN_POINT('Ctrl Pts',(43.4753311640868,21.3750000013656,-104.958734125));
#8236=CARTESIAN_POINT('Ctrl Pts',(74.2170326445434,21.3125000013656,-74.2170326445434));
#8237=CARTESIAN_POINT('Ctrl Pts',(104.958734125,21.2500000013656,-43.4753311640868));
#8238=CARTESIAN_POINT('Ctrl Pts',(104.958734125,21.1875000013656,-1.28537377788739E-14));
#8239=CARTESIAN_POINT('Ctrl Pts',(104.958734125,21.1250000013656,43.4753311640868));
#8240=CARTESIAN_POINT('Ctrl Pts',(74.2170326445434,21.0625000013656,74.2170326445434));
#8241=CARTESIAN_POINT('Ctrl Pts',(43.4753311640869,21.0000000013656,104.958734125));
#8242=CARTESIAN_POINT('Ctrl Pts',(1.92806066683109E-14,20.9375000013656,
104.958734125));
#8243=CARTESIAN_POINT('Ctrl Pts',(-43.4753311640868,20.8750000013656,104.958734125));
#8244=CARTESIAN_POINT('Ctrl Pts',(-74.2170326445434,20.8125000013656,74.2170326445434));
#8245=CARTESIAN_POINT('Ctrl Pts',(-104.958734125,20.7500000013656,43.4753311640869));
#8246=CARTESIAN_POINT('Ctrl Pts',(-104.958734125,20.6875000013656,0.));
#8247=CARTESIAN_POINT('Ctrl Pts',(-104.958734125,20.6250000013656,-43.4753311640868));
#8248=CARTESIAN_POINT('Ctrl Pts',(-74.2170326445434,20.5625000013656,-74.2170326445434));
#8249=CARTESIAN_POINT('Ctrl Pts',(-43.4753311640868,20.5000000013656,-104.958734125));
#8250=CARTESIAN_POINT('Ctrl Pts',(-6.42686888943697E-15,20.4375000013656,
-104.958734125));
#8251=CARTESIAN_POINT('Ctrl Pts',(43.4753311640868,20.3750000013656,-104.958734125));
#8252=CARTESIAN_POINT('Ctrl Pts',(74.2170326445434,20.3125000013656,-74.2170326445434));
#8253=CARTESIAN_POINT('Ctrl Pts',(104.958734125,20.2500000013656,-43.4753311640868));
#8254=CARTESIAN_POINT('Ctrl Pts',(104.958734125,20.1875000013656,-1.28537377788739E-14));
#8255=CARTESIAN_POINT('Ctrl Pts',(104.958734125,20.1250000013656,43.4753311640868));
#8256=CARTESIAN_POINT('Ctrl Pts',(74.2170326445434,20.0625000013656,74.2170326445434));
#8257=CARTESIAN_POINT('Ctrl Pts',(43.4753311640869,20.0000000013656,104.958734125));
#8258=CARTESIAN_POINT('Ctrl Pts',(1.92806066683109E-14,19.9375000013656,
104.958734125));
#8259=CARTESIAN_POINT('Ctrl Pts',(-43.4753311640868,19.8750000013656,104.958734125));
#8260=CARTESIAN_POINT('Ctrl Pts',(-74.2170326445434,19.8125000013656,74.2170326445434));
#8261=CARTESIAN_POINT('Ctrl Pts',(-104.958734125,19.7500000013656,43.4753311640869));
#8262=CARTESIAN_POINT('Ctrl Pts',(-104.958734125,19.6875000013656,0.));
#8263=CARTESIAN_POINT('Ctrl Pts',(-104.958734125,19.6250000013656,-43.4753311640868));
#8264=CARTESIAN_POINT('Ctrl Pts',(-74.2170326445434,19.5625000013656,-74.2170326445434));
#8265=CARTESIAN_POINT('Ctrl Pts',(-43.4753311640868,19.5000000013656,-104.958734125));
#8266=CARTESIAN_POINT('Ctrl Pts',(-6.42686888943697E-15,19.4375000013656,
-104.958734125));
#8267=CARTESIAN_POINT('Ctrl Pts',(43.4753311640868,19.3750000013656,-104.958734125));
#8268=CARTESIAN_POINT('Ctrl Pts',(74.2170326445434,19.3125000013656,-74.2170326445434));
#8269=CARTESIAN_POINT('Ctrl Pts',(104.958734125,19.2500000013656,-43.4753311640868));
#8270=CARTESIAN_POINT('Ctrl Pts',(104.958734125,19.1875000013656,-1.28537377788739E-14));
#8271=CARTESIAN_POINT('Ctrl Pts',(104.958734125,19.1250000013656,43.4753311640868));
#8272=CARTESIAN_POINT('Ctrl Pts',(74.2170326445434,19.0625000013656,74.2170326445434));
#8273=CARTESIAN_POINT('Ctrl Pts',(43.4753311640869,19.0000000013656,104.958734125));
#8274=CARTESIAN_POINT('Ctrl Pts',(1.92806066683109E-14,18.9375000013656,
104.958734125));
#8275=CARTESIAN_POINT('Ctrl Pts',(-43.4753311640868,18.8750000013656,104.958734125));
#8276=CARTESIAN_POINT('Ctrl Pts',(-74.2170326445434,18.8125000013656,74.2170326445434));
#8277=CARTESIAN_POINT('Ctrl Pts',(-104.958734125,18.7500000013656,43.4753311640869));
#8278=CARTESIAN_POINT('Ctrl Pts',(-104.958734125,18.6875000013656,0.));
#8279=CARTESIAN_POINT('Ctrl Pts',(-104.958734125,18.6250000013656,-43.4753311640868));
#8280=CARTESIAN_POINT('Ctrl Pts',(-74.2170326445434,18.5625000013656,-74.2170326445434));
#8281=CARTESIAN_POINT('Ctrl Pts',(-43.4753311640868,18.5000000013656,-104.958734125));
#8282=CARTESIAN_POINT('Ctrl Pts',(-6.42686888943697E-15,18.4375000013656,
-104.958734125));
#8283=CARTESIAN_POINT('Ctrl Pts',(43.4753311640868,18.3750000013656,-104.958734125));
#8284=CARTESIAN_POINT('Ctrl Pts',(74.2170326445434,18.3125000013656,-74.2170326445434));
#8285=CARTESIAN_POINT('Ctrl Pts',(104.958734125,18.2500000013656,-43.4753311640868));
#8286=CARTESIAN_POINT('Ctrl Pts',(104.958734125,18.1875000013656,-1.28537377788739E-14));
#8287=CARTESIAN_POINT('Ctrl Pts',(104.958734125,18.1250000013656,43.4753311640868));
#8288=CARTESIAN_POINT('Ctrl Pts',(74.2170326445434,18.0625000013656,74.2170326445434));
#8289=CARTESIAN_POINT('Ctrl Pts',(43.4753311640869,18.0000000013656,104.958734125));
#8290=CARTESIAN_POINT('Ctrl Pts',(1.92806066683109E-14,17.9375000013656,
104.958734125));
#8291=CARTESIAN_POINT('Ctrl Pts',(-43.4753311640868,17.8750000013656,104.958734125));
#8292=CARTESIAN_POINT('Ctrl Pts',(-74.2170326445434,17.8125000013656,74.2170326445434));
#8293=CARTESIAN_POINT('Ctrl Pts',(-104.958734125,17.7500000013656,43.4753311640869));
#8294=CARTESIAN_POINT('Ctrl Pts',(-104.958734125,17.6875000013656,0.));
#8295=CARTESIAN_POINT('Ctrl Pts',(-104.958734125,17.6250000013656,-43.4753311640868));
#8296=CARTESIAN_POINT('Ctrl Pts',(-74.2170326445434,17.5625000013656,-74.2170326445434));
#8297=CARTESIAN_POINT('Ctrl Pts',(-43.4753311640868,17.5000000013656,-104.958734125));
#8298=CARTESIAN_POINT('Ctrl Pts',(-6.42686888943697E-15,17.4375000013656,
-104.958734125));
#8299=CARTESIAN_POINT('Ctrl Pts',(43.4753311640868,17.3750000013656,-104.958734125));
#8300=CARTESIAN_POINT('Ctrl Pts',(74.2170326445434,17.3125000013656,-74.2170326445434));
#8301=CARTESIAN_POINT('Ctrl Pts',(104.958734125,17.2500000013656,-43.4753311640868));
#8302=CARTESIAN_POINT('Ctrl Pts',(104.958734125,17.1875000013656,-1.28537377788739E-14));
#8303=CARTESIAN_POINT('Ctrl Pts',(104.958734125,17.1250000013656,43.4753311640868));
#8304=CARTESIAN_POINT('Ctrl Pts',(74.2170326445434,17.0625000013656,74.2170326445434));
#8305=CARTESIAN_POINT('Ctrl Pts',(43.4753311640869,17.0000000013656,104.958734125));
#8306=CARTESIAN_POINT('Ctrl Pts',(1.92806066683109E-14,16.9375000013656,
104.958734125));
#8307=CARTESIAN_POINT('Ctrl Pts',(-43.4753311640868,16.8750000013656,104.958734125));
#8308=CARTESIAN_POINT('Ctrl Pts',(-74.2170326445434,16.8125000013656,74.2170326445434));
#8309=CARTESIAN_POINT('Ctrl Pts',(-104.958734125,16.7500000013656,43.4753311640869));
#8310=CARTESIAN_POINT('Ctrl Pts',(-104.958734125,16.6875000013656,0.));
#8311=CARTESIAN_POINT('Ctrl Pts',(-104.958734125,16.6250000013656,-43.4753311640868));
#8312=CARTESIAN_POINT('Ctrl Pts',(-74.2170326445434,16.5625000013656,-74.2170326445434));
#8313=CARTESIAN_POINT('Ctrl Pts',(-43.4753311640868,16.5000000013656,-104.958734125));
#8314=CARTESIAN_POINT('Ctrl Pts',(-6.42686888943697E-15,16.4375000013656,
-104.958734125));
#8315=CARTESIAN_POINT('Ctrl Pts',(43.4753311640868,16.3750000013656,-104.958734125));
#8316=CARTESIAN_POINT('Ctrl Pts',(74.2170326445434,16.3125000013656,-74.2170326445434));
#8317=CARTESIAN_POINT('Ctrl Pts',(104.958734125,16.2500000013656,-43.4753311640868));
#8318=CARTESIAN_POINT('Ctrl Pts',(104.958734125,16.1875000013656,-1.28537377788739E-14));
#8319=CARTESIAN_POINT('Ctrl Pts',(104.958734125,16.1250000013656,43.4753311640868));
#8320=CARTESIAN_POINT('Ctrl Pts',(74.2170326445434,16.0625000013656,74.2170326445434));
#8321=CARTESIAN_POINT('Ctrl Pts',(43.4753311640869,16.0000000013656,104.958734125));
#8322=CARTESIAN_POINT('Ctrl Pts',(1.92806066683109E-14,15.9375000013656,
104.958734125));
#8323=CARTESIAN_POINT('Ctrl Pts',(-43.4753311640868,15.8750000013656,104.958734125));
#8324=CARTESIAN_POINT('Ctrl Pts',(-74.2170326445434,15.8125000013656,74.2170326445434));
#8325=CARTESIAN_POINT('Ctrl Pts',(-104.958734125,15.7500000013656,43.4753311640869));
#8326=CARTESIAN_POINT('Ctrl Pts',(-104.958734125,15.6875000013656,0.));
#8327=CARTESIAN_POINT('Ctrl Pts',(-104.958734125,15.6250000013656,-43.4753311640868));
#8328=CARTESIAN_POINT('Ctrl Pts',(-74.2170326445434,15.5625000013656,-74.2170326445434));
#8329=CARTESIAN_POINT('Ctrl Pts',(-43.4753311640868,15.5000000013656,-104.958734125));
#8330=CARTESIAN_POINT('Ctrl Pts',(-6.42686888943697E-15,15.4375000013656,
-104.958734125));
#8331=CARTESIAN_POINT('Ctrl Pts',(43.4753311640868,15.3750000013656,-104.958734125));
#8332=CARTESIAN_POINT('Ctrl Pts',(74.2170326445434,15.3125000013656,-74.2170326445434));
#8333=CARTESIAN_POINT('Ctrl Pts',(104.958734125,15.2500000013656,-43.4753311640868));
#8334=CARTESIAN_POINT('Ctrl Pts',(104.958734125,15.1875000013656,-1.28537377788739E-14));
#8335=CARTESIAN_POINT('Ctrl Pts',(104.958734125,15.1250000013656,43.4753311640868));
#8336=CARTESIAN_POINT('Ctrl Pts',(74.2170326445434,15.0625000013656,74.2170326445434));
#8337=CARTESIAN_POINT('Ctrl Pts',(43.4753311640869,15.0000000013656,104.958734125));
#8338=CARTESIAN_POINT('Ctrl Pts',(1.92806066683109E-14,14.9375000013656,
104.958734125));
#8339=CARTESIAN_POINT('Ctrl Pts',(-43.4753311640868,14.8750000013656,104.958734125));
#8340=CARTESIAN_POINT('Ctrl Pts',(-74.2170326445434,14.8125000013656,74.2170326445434));
#8341=CARTESIAN_POINT('Ctrl Pts',(-104.958734125,14.7500000013656,43.4753311640869));
#8342=CARTESIAN_POINT('Ctrl Pts',(-104.958734125,14.6875000013656,0.));
#8343=CARTESIAN_POINT('Ctrl Pts',(-104.958734125,14.6250000013656,-43.4753311640868));
#8344=CARTESIAN_POINT('Ctrl Pts',(-74.2170326445434,14.5625000013656,-74.2170326445434));
#8345=CARTESIAN_POINT('Ctrl Pts',(-43.4753311640868,14.5000000013656,-104.958734125));
#8346=CARTESIAN_POINT('Ctrl Pts',(-6.42686888943697E-15,14.4375000013656,
-104.958734125));
#8347=CARTESIAN_POINT('Ctrl Pts',(43.4753311640868,14.3750000013656,-104.958734125));
#8348=CARTESIAN_POINT('Ctrl Pts',(74.2170326445434,14.3125000013656,-74.2170326445434));
#8349=CARTESIAN_POINT('Ctrl Pts',(104.958734125,14.2500000013656,-43.4753311640868));
#8350=CARTESIAN_POINT('Ctrl Pts',(104.958734125,14.1875000013656,-1.28537377788739E-14));
#8351=CARTESIAN_POINT('Ctrl Pts',(104.958734125,14.1250000013656,43.4753311640868));
#8352=CARTESIAN_POINT('Ctrl Pts',(74.2170326445434,14.0625000013656,74.2170326445434));
#8353=CARTESIAN_POINT('Ctrl Pts',(43.4753311640869,14.0000000013656,104.958734125));
#8354=CARTESIAN_POINT('Ctrl Pts',(1.92806066683109E-14,13.9375000013656,
104.958734125));
#8355=CARTESIAN_POINT('Ctrl Pts',(-43.4753311640868,13.8750000013656,104.958734125));
#8356=CARTESIAN_POINT('Ctrl Pts',(-74.2170326445434,13.8125000013656,74.2170326445434));
#8357=CARTESIAN_POINT('Ctrl Pts',(-104.958734125,13.7500000013656,43.4753311640869));
#8358=CARTESIAN_POINT('Ctrl Pts',(-104.958734125,13.6875000013656,0.));
#8359=CARTESIAN_POINT('Ctrl Pts',(-104.958734125,13.6250000013656,-43.4753311640868));
#8360=CARTESIAN_POINT('Ctrl Pts',(-74.2170326445434,13.5625000013656,-74.2170326445434));
#8361=CARTESIAN_POINT('Ctrl Pts',(-43.4753311640868,13.5000000013656,-104.958734125));
#8362=CARTESIAN_POINT('Ctrl Pts',(-6.42686888943697E-15,13.4375000013656,
-104.958734125));
#8363=CARTESIAN_POINT('Ctrl Pts',(43.4753311640868,13.3750000013656,-104.958734125));
#8364=CARTESIAN_POINT('Ctrl Pts',(74.2170326445434,13.3125000013656,-74.2170326445434));
#8365=CARTESIAN_POINT('Ctrl Pts',(104.958734125,13.2500000013656,-43.4753311640868));
#8366=CARTESIAN_POINT('Ctrl Pts',(104.958734125,13.1875000013656,-1.28537377788739E-14));
#8367=CARTESIAN_POINT('Ctrl Pts',(104.958734125,13.1250000013656,43.4753311640868));
#8368=CARTESIAN_POINT('Ctrl Pts',(74.2170326445434,13.0625000013656,74.2170326445434));
#8369=CARTESIAN_POINT('Ctrl Pts',(43.4753311640869,13.0000000013656,104.958734125));
#8370=CARTESIAN_POINT('Ctrl Pts',(1.92806066683109E-14,12.9375000013656,
104.958734125));
#8371=CARTESIAN_POINT('Ctrl Pts',(-43.4753311640868,12.8750000013656,104.958734125));
#8372=CARTESIAN_POINT('Ctrl Pts',(-74.2170326445434,12.8125000013656,74.2170326445434));
#8373=CARTESIAN_POINT('Ctrl Pts',(-104.958734125,12.7500000013656,43.4753311640869));
#8374=CARTESIAN_POINT('Ctrl Pts',(-104.958734125,12.6875000013656,0.));
#8375=CARTESIAN_POINT('Ctrl Pts',(-104.958734125,12.6250000013656,-43.4753311640868));
#8376=CARTESIAN_POINT('Ctrl Pts',(-74.2170326445434,12.5625000013656,-74.2170326445434));
#8377=CARTESIAN_POINT('Ctrl Pts',(-43.4753311640868,12.5000000013656,-104.958734125));
#8378=CARTESIAN_POINT('Ctrl Pts',(-6.42686888943697E-15,12.4375000013656,
-104.958734125));
#8379=CARTESIAN_POINT('Ctrl Pts',(43.4753311640868,12.3750000013656,-104.958734125));
#8380=CARTESIAN_POINT('Ctrl Pts',(74.2170326445434,12.3125000013656,-74.2170326445434));
#8381=CARTESIAN_POINT('Ctrl Pts',(104.958734125,12.2500000013656,-43.4753311640868));
#8382=CARTESIAN_POINT('Ctrl Pts',(104.958734125,12.1875000013656,-1.28537377788739E-14));
#8383=CARTESIAN_POINT('Ctrl Pts',(104.958734125,12.1250000013656,43.4753311640868));
#8384=CARTESIAN_POINT('Ctrl Pts',(74.2170326445434,12.0625000013656,74.2170326445434));
#8385=CARTESIAN_POINT('Ctrl Pts',(43.4753311640869,12.0000000013656,104.958734125));
#8386=CARTESIAN_POINT('Ctrl Pts',(1.92806066683109E-14,11.9375000013656,
104.958734125));
#8387=CARTESIAN_POINT('Ctrl Pts',(-43.4753311640868,11.8750000013656,104.958734125));
#8388=CARTESIAN_POINT('Ctrl Pts',(-74.2170326445434,11.8125000013656,74.2170326445434));
#8389=CARTESIAN_POINT('Ctrl Pts',(-104.958734125,11.7500000013656,43.4753311640869));
#8390=CARTESIAN_POINT('Ctrl Pts',(-104.958734125,11.6875000013656,0.));
#8391=CARTESIAN_POINT('Ctrl Pts',(-104.958734125,11.6250000013656,-43.4753311640868));
#8392=CARTESIAN_POINT('Ctrl Pts',(-74.2170326445434,11.5625000013656,-74.2170326445434));
#8393=CARTESIAN_POINT('Ctrl Pts',(-43.4753311640868,11.5000000013656,-104.958734125));
#8394=CARTESIAN_POINT('Ctrl Pts',(-6.42686888943697E-15,11.4375000013656,
-104.958734125));
#8395=CARTESIAN_POINT('Ctrl Pts',(43.4753311640868,11.3750000013656,-104.958734125));
#8396=CARTESIAN_POINT('Ctrl Pts',(74.2170326445434,11.3125000013656,-74.2170326445434));
#8397=CARTESIAN_POINT('Ctrl Pts',(104.958734125,11.2500000013656,-43.4753311640868));
#8398=CARTESIAN_POINT('Ctrl Pts',(104.958734125,11.1875000013656,-1.28537377788739E-14));
#8399=CARTESIAN_POINT('Ctrl Pts',(104.958734125,11.1250000013656,43.4753311640868));
#8400=CARTESIAN_POINT('Ctrl Pts',(74.2170326445434,11.0625000013656,74.2170326445434));
#8401=CARTESIAN_POINT('Ctrl Pts',(43.4753311640869,11.0000000013656,104.958734125));
#8402=CARTESIAN_POINT('Ctrl Pts',(1.92806066683109E-14,10.9375000013656,
104.958734125));
#8403=CARTESIAN_POINT('Ctrl Pts',(-43.4753311640868,10.8750000013656,104.958734125));
#8404=CARTESIAN_POINT('Ctrl Pts',(-74.2170326445434,10.8125000013656,74.2170326445434));
#8405=CARTESIAN_POINT('Ctrl Pts',(-104.958734125,10.7500000013656,43.4753311640869));
#8406=CARTESIAN_POINT('Ctrl Pts',(-104.958734125,10.6875000013656,0.));
#8407=CARTESIAN_POINT('Ctrl Pts',(-104.958734125,10.6250000013656,-43.4753311640868));
#8408=CARTESIAN_POINT('Ctrl Pts',(-74.2170326445434,10.5625000013656,-74.2170326445434));
#8409=CARTESIAN_POINT('Ctrl Pts',(-43.4753311640868,10.5000000013656,-104.958734125));
#8410=CARTESIAN_POINT('Ctrl Pts',(-6.42686888943697E-15,10.4375000013656,
-104.958734125));
#8411=CARTESIAN_POINT('Ctrl Pts',(43.4753311640868,10.3750000013656,-104.958734125));
#8412=CARTESIAN_POINT('Ctrl Pts',(74.2170326445434,10.3125000013656,-74.2170326445434));
#8413=CARTESIAN_POINT('Ctrl Pts',(104.958734125,10.2500000013656,-43.4753311640868));
#8414=CARTESIAN_POINT('Ctrl Pts',(104.958734125,10.1875000013656,-1.28537377788739E-14));
#8415=CARTESIAN_POINT('Ctrl Pts',(104.958734125,10.1250000013656,43.4753311640868));
#8416=CARTESIAN_POINT('Ctrl Pts',(74.2170326445434,10.0625000013656,74.2170326445434));
#8417=CARTESIAN_POINT('Ctrl Pts',(43.4753311640869,10.0000000013656,104.958734125));
#8418=CARTESIAN_POINT('Ctrl Pts',(1.92806066683109E-14,9.93750000136558,
104.958734125));
#8419=CARTESIAN_POINT('Ctrl Pts',(-43.4753311640868,9.87500000136558,104.958734125));
#8420=CARTESIAN_POINT('Ctrl Pts',(-74.2170326445434,9.81250000136558,74.2170326445434));
#8421=CARTESIAN_POINT('Ctrl Pts',(-104.958734125,9.75000000136558,43.4753311640869));
#8422=CARTESIAN_POINT('Ctrl Pts',(-104.958734125,9.68750000136558,0.));
#8423=CARTESIAN_POINT('Ctrl Pts',(-104.958734125,9.62500000136558,-43.4753311640868));
#8424=CARTESIAN_POINT('Ctrl Pts',(-74.2170326445434,9.56250000136558,-74.2170326445434));
#8425=CARTESIAN_POINT('Ctrl Pts',(-43.4753311640868,9.50000000136558,-104.958734125));
#8426=CARTESIAN_POINT('Ctrl Pts',(-6.42686888943697E-15,9.43750000136558,
-104.958734125));
#8427=CARTESIAN_POINT('Ctrl Pts',(43.4753311640868,9.37500000136558,-104.958734125));
#8428=CARTESIAN_POINT('Ctrl Pts',(74.2170326445434,9.31250000136558,-74.2170326445434));
#8429=CARTESIAN_POINT('Ctrl Pts',(104.958734125,9.25000000136558,-43.4753311640868));
#8430=CARTESIAN_POINT('Ctrl Pts',(104.958734125,9.18750000136558,-1.28537377788739E-14));
#8431=CARTESIAN_POINT('Ctrl Pts',(104.958734125,9.12500000136558,43.4753311640868));
#8432=CARTESIAN_POINT('Ctrl Pts',(74.2170326445434,9.06250000136558,74.2170326445434));
#8433=CARTESIAN_POINT('Ctrl Pts',(43.4753311640869,9.00000000136558,104.958734125));
#8434=CARTESIAN_POINT('Ctrl Pts',(1.92806066683109E-14,8.93750000136558,
104.958734125));
#8435=CARTESIAN_POINT('Ctrl Pts',(-43.4753311640868,8.87500000136558,104.958734125));
#8436=CARTESIAN_POINT('Ctrl Pts',(-74.2170326445434,8.81250000136558,74.2170326445434));
#8437=CARTESIAN_POINT('Ctrl Pts',(-104.958734125,8.75000000136558,43.4753311640869));
#8438=CARTESIAN_POINT('Ctrl Pts',(-104.958734125,8.68750000136558,0.));
#8439=CARTESIAN_POINT('Ctrl Pts',(-104.958734125,8.62500000136558,-43.4753311640868));
#8440=CARTESIAN_POINT('Ctrl Pts',(-74.2170326445434,8.56250000136558,-74.2170326445434));
#8441=CARTESIAN_POINT('Ctrl Pts',(-43.4753311640868,8.50000000136558,-104.958734125));
#8442=CARTESIAN_POINT('Ctrl Pts',(-6.42686888943697E-15,8.43750000136558,
-104.958734125));
#8443=CARTESIAN_POINT('Ctrl Pts',(43.4753311640868,8.37500000136558,-104.958734125));
#8444=CARTESIAN_POINT('Ctrl Pts',(74.2170326445434,8.31250000136558,-74.2170326445434));
#8445=CARTESIAN_POINT('Ctrl Pts',(104.958734125,8.25000000136558,-43.4753311640868));
#8446=CARTESIAN_POINT('Ctrl Pts',(104.958734125,8.18750000136558,-1.28537377788739E-14));
#8447=CARTESIAN_POINT('Ctrl Pts',(104.958734125,8.12500000136558,43.4753311640868));
#8448=CARTESIAN_POINT('Ctrl Pts',(74.2170326445434,8.06250000136558,74.2170326445434));
#8449=CARTESIAN_POINT('Ctrl Pts',(43.4753311640869,8.00000000136558,104.958734125));
#8450=CARTESIAN_POINT('Ctrl Pts',(1.92806066683109E-14,7.93750000136558,
104.958734125));
#8451=CARTESIAN_POINT('Ctrl Pts',(-43.4753311640868,7.87500000136558,104.958734125));
#8452=CARTESIAN_POINT('Ctrl Pts',(-74.2170326445434,7.81250000136558,74.2170326445434));
#8453=CARTESIAN_POINT('Ctrl Pts',(-104.958734125,7.75000000136558,43.4753311640869));
#8454=CARTESIAN_POINT('Ctrl Pts',(-104.958734125,7.68750000136558,0.));
#8455=CARTESIAN_POINT('Ctrl Pts',(-104.958734125,7.62500000136558,-43.4753311640868));
#8456=CARTESIAN_POINT('Ctrl Pts',(-74.2170326445434,7.56250000136558,-74.2170326445434));
#8457=CARTESIAN_POINT('Ctrl Pts',(-43.4753311640868,7.50000000136558,-104.958734125));
#8458=CARTESIAN_POINT('Ctrl Pts',(-6.42686888943697E-15,7.43750000136558,
-104.958734125));
#8459=CARTESIAN_POINT('Ctrl Pts',(43.4753311640868,7.37500000136558,-104.958734125));
#8460=CARTESIAN_POINT('Ctrl Pts',(74.2170326445434,7.31250000136558,-74.2170326445434));
#8461=CARTESIAN_POINT('Ctrl Pts',(104.958734125,7.25000000136558,-43.4753311640868));
#8462=CARTESIAN_POINT('Ctrl Pts',(104.958734125,7.18750000136558,-1.28537377788739E-14));
#8463=CARTESIAN_POINT('Ctrl Pts',(104.958734125,7.12500000136558,43.4753311640868));
#8464=CARTESIAN_POINT('Ctrl Pts',(74.2170326445434,7.06250000136558,74.2170326445434));
#8465=CARTESIAN_POINT('Ctrl Pts',(43.4753311640869,7.00000000136558,104.958734125));
#8466=CARTESIAN_POINT('Ctrl Pts',(1.92806066683109E-14,6.93750000136558,
104.958734125));
#8467=CARTESIAN_POINT('Ctrl Pts',(-43.4753311640868,6.87500000136558,104.958734125));
#8468=CARTESIAN_POINT('Ctrl Pts',(-74.2170326445434,6.81250000136558,74.2170326445434));
#8469=CARTESIAN_POINT('Ctrl Pts',(-104.958734125,6.75000000136558,43.4753311640869));
#8470=CARTESIAN_POINT('Ctrl Pts',(-104.958734125,6.68750000136558,0.));
#8471=CARTESIAN_POINT('Ctrl Pts',(-104.958734125,6.62500000136558,-43.4753311640868));
#8472=CARTESIAN_POINT('Ctrl Pts',(-74.2170326445434,6.56250000136558,-74.2170326445434));
#8473=CARTESIAN_POINT('Ctrl Pts',(-43.4753311640868,6.50000000136558,-104.958734125));
#8474=CARTESIAN_POINT('Ctrl Pts',(-6.42686888943697E-15,6.43750000136558,
-104.958734125));
#8475=CARTESIAN_POINT('Ctrl Pts',(43.4753311640868,6.37500000136558,-104.958734125));
#8476=CARTESIAN_POINT('Ctrl Pts',(74.2170326445434,6.31250000136558,-74.2170326445434));
#8477=CARTESIAN_POINT('Ctrl Pts',(104.958734125,6.25000000136558,-43.4753311640868));
#8478=CARTESIAN_POINT('Ctrl Pts',(104.958734125,6.18750000136558,-1.28537377788739E-14));
#8479=CARTESIAN_POINT('Ctrl Pts',(104.958734125,6.12500000136558,43.4753311640868));
#8480=CARTESIAN_POINT('Ctrl Pts',(74.2170326445434,6.06250000136558,74.2170326445434));
#8481=CARTESIAN_POINT('Ctrl Pts',(43.4753311640869,6.00000000136558,104.958734125));
#8482=CARTESIAN_POINT('Ctrl Pts',(1.92806066683109E-14,5.93750000136558,
104.958734125));
#8483=CARTESIAN_POINT('Ctrl Pts',(-43.4753311640868,5.87500000136558,104.958734125));
#8484=CARTESIAN_POINT('Ctrl Pts',(-74.2170326445434,5.81250000136558,74.2170326445434));
#8485=CARTESIAN_POINT('Ctrl Pts',(-104.958734125,5.75000000136558,43.4753311640869));
#8486=CARTESIAN_POINT('Ctrl Pts',(-104.958734125,5.68750000136559,0.));
#8487=CARTESIAN_POINT('Ctrl Pts',(-104.958734125,5.62500000136559,-43.4753311640868));
#8488=CARTESIAN_POINT('Ctrl Pts',(-74.2170326445434,5.56250000136559,-74.2170326445434));
#8489=CARTESIAN_POINT('Ctrl Pts',(-43.4753311640868,5.50000000136559,-104.958734125));
#8490=CARTESIAN_POINT('Ctrl Pts',(-6.42686888943697E-15,5.43750000136559,
-104.958734125));
#8491=CARTESIAN_POINT('Ctrl Pts',(43.4753311640868,5.37500000136559,-104.958734125));
#8492=CARTESIAN_POINT('Ctrl Pts',(74.2170326445434,5.31250000136558,-74.2170326445434));
#8493=CARTESIAN_POINT('Ctrl Pts',(104.958734125,5.25000000136559,-43.4753311640868));
#8494=CARTESIAN_POINT('Ctrl Pts',(104.958734125,5.18750000136559,-1.28537377788739E-14));
#8495=CARTESIAN_POINT('Ctrl Pts',(104.958734125,5.12500000136559,43.4753311640868));
#8496=CARTESIAN_POINT('Ctrl Pts',(74.2170326445434,5.06250000136559,74.2170326445434));
#8497=CARTESIAN_POINT('Ctrl Pts',(43.4753311640869,5.00000000136558,104.958734125));
#8498=CARTESIAN_POINT('Ctrl Pts',(1.92806066683109E-14,4.93750000136559,
104.958734125));
#8499=CARTESIAN_POINT('Ctrl Pts',(-43.4753311640868,4.87500000136559,104.958734125));
#8500=CARTESIAN_POINT('Ctrl Pts',(-74.2170326445434,4.81250000136559,74.2170326445434));
#8501=CARTESIAN_POINT('Ctrl Pts',(-104.958734125,4.75000000136558,43.4753311640869));
#8502=CARTESIAN_POINT('Ctrl Pts',(-104.958734125,4.68750000136558,0.));
#8503=CARTESIAN_POINT('Ctrl Pts',(-104.958734125,4.62500000136559,-43.4753311640868));
#8504=CARTESIAN_POINT('Ctrl Pts',(-74.2170326445434,4.56250000136558,-74.2170326445434));
#8505=CARTESIAN_POINT('Ctrl Pts',(-43.4753311640868,4.50000000136558,-104.958734125));
#8506=CARTESIAN_POINT('Ctrl Pts',(-6.42686888943697E-15,4.43750000136558,
-104.958734125));
#8507=CARTESIAN_POINT('Ctrl Pts',(43.4753311640868,4.37500000136558,-104.958734125));
#8508=CARTESIAN_POINT('Ctrl Pts',(74.2170326445434,4.31250000136558,-74.2170326445434));
#8509=CARTESIAN_POINT('Ctrl Pts',(104.958734125,4.25000000136558,-43.4753311640868));
#8510=CARTESIAN_POINT('Ctrl Pts',(104.958734125,4.18750000136558,-1.28537377788739E-14));
#8511=CARTESIAN_POINT('Ctrl Pts',(104.958734125,4.12500000136558,43.4753311640868));
#8512=CARTESIAN_POINT('Ctrl Pts',(74.2170326445434,4.06250000136558,74.2170326445434));
#8513=CARTESIAN_POINT('Ctrl Pts',(43.4753311640869,4.00000000136558,104.958734125));
#8514=CARTESIAN_POINT('Ctrl Pts',(1.92806066683109E-14,3.93750000136558,
104.958734125));
#8515=CARTESIAN_POINT('Ctrl Pts',(-43.4753311640868,3.87500000136558,104.958734125));
#8516=CARTESIAN_POINT('Ctrl Pts',(-74.2170326445434,3.81250000136558,74.2170326445434));
#8517=CARTESIAN_POINT('Ctrl Pts',(-104.958734125,3.75000000136558,43.4753311640869));
#8518=CARTESIAN_POINT('Ctrl Pts',(-104.958734125,3.68750000136558,0.));
#8519=CARTESIAN_POINT('Ctrl Pts',(-104.958734125,3.62500000136558,-43.4753311640868));
#8520=CARTESIAN_POINT('Ctrl Pts',(-74.2170326445434,3.56250000136558,-74.2170326445434));
#8521=CARTESIAN_POINT('Ctrl Pts',(-43.4753311640868,3.50000000136558,-104.958734125));
#8522=CARTESIAN_POINT('Ctrl Pts',(-6.42686888943697E-15,3.43750000136558,
-104.958734125));
#8523=CARTESIAN_POINT('Ctrl Pts',(43.4753311640868,3.37500000136558,-104.958734125));
#8524=CARTESIAN_POINT('Ctrl Pts',(74.2170326445434,3.31250000136558,-74.2170326445434));
#8525=CARTESIAN_POINT('Ctrl Pts',(104.958734125,3.25000000136558,-43.4753311640868));
#8526=CARTESIAN_POINT('Ctrl Pts',(104.958734125,3.18750000136558,-1.28537377788739E-14));
#8527=CARTESIAN_POINT('Ctrl Pts',(104.958734125,3.12500000136558,43.4753311640868));
#8528=CARTESIAN_POINT('Ctrl Pts',(74.2170326445434,3.06250000136558,74.2170326445434));
#8529=CARTESIAN_POINT('Ctrl Pts',(43.4753311640869,3.00000000136558,104.958734125));
#8530=CARTESIAN_POINT('Ctrl Pts',(1.92806066683109E-14,2.93750000136558,
104.958734125));
#8531=CARTESIAN_POINT('Ctrl Pts',(-43.4753311640868,2.87500000136558,104.958734125));
#8532=CARTESIAN_POINT('Ctrl Pts',(-74.2170326445434,2.81250000136558,74.2170326445434));
#8533=CARTESIAN_POINT('Ctrl Pts',(-104.958734125,2.75000000136558,43.4753311640869));
#8534=CARTESIAN_POINT('Ctrl Pts',(-104.958734125,2.68750000136558,0.));
#8535=CARTESIAN_POINT('Ctrl Pts',(-104.958734125,2.62500000136558,-43.4753311640868));
#8536=CARTESIAN_POINT('Ctrl Pts',(-74.2170326445434,2.56250000136558,-74.2170326445434));
#8537=CARTESIAN_POINT('Ctrl Pts',(-43.4753311640868,2.50000000136558,-104.958734125));
#8538=CARTESIAN_POINT('Ctrl Pts',(-6.42686888943697E-15,2.43750000136558,
-104.958734125));
#8539=CARTESIAN_POINT('Ctrl Pts',(43.4753311640868,2.37500000136558,-104.958734125));
#8540=CARTESIAN_POINT('Ctrl Pts',(74.2170326445434,2.31250000136558,-74.2170326445434));
#8541=CARTESIAN_POINT('Ctrl Pts',(104.958734125,2.25000000136558,-43.4753311640868));
#8542=CARTESIAN_POINT('Ctrl Pts',(104.958734125,2.18750000136558,-1.28537377788739E-14));
#8543=CARTESIAN_POINT('Ctrl Pts',(104.958734125,2.12500000136558,43.4753311640868));
#8544=CARTESIAN_POINT('Ctrl Pts',(74.2170326445434,2.06250000136558,74.2170326445434));
#8545=CARTESIAN_POINT('Ctrl Pts',(43.4753311640869,2.00000000136558,104.958734125));
#8546=CARTESIAN_POINT('Ctrl Pts',(1.92806066683109E-14,1.93750000136558,
104.958734125));
#8547=CARTESIAN_POINT('Ctrl Pts',(-43.4753311640868,1.87500000136558,104.958734125));
#8548=CARTESIAN_POINT('Ctrl Pts',(-74.2170326445434,1.81250000136558,74.2170326445434));
#8549=CARTESIAN_POINT('Ctrl Pts',(-104.958734125,1.75000000136558,43.4753311640869));
#8550=CARTESIAN_POINT('Ctrl Pts',(-104.958734125,1.68750000136558,0.));
#8551=CARTESIAN_POINT('Ctrl Pts',(-104.958734125,1.62500000136558,-43.4753311640868));
#8552=CARTESIAN_POINT('Ctrl Pts',(-74.2170326445434,1.56250000136558,-74.2170326445434));
#8553=CARTESIAN_POINT('Ctrl Pts',(-43.4753311640868,1.50000000136558,-104.958734125));
#8554=CARTESIAN_POINT('Ctrl Pts',(-6.42686888943697E-15,1.43750000136558,
-104.958734125));
#8555=CARTESIAN_POINT('Ctrl Pts',(43.4753311640868,1.37500000136558,-104.958734125));
#8556=CARTESIAN_POINT('Ctrl Pts',(74.2170326445434,1.31250000136558,-74.2170326445434));
#8557=CARTESIAN_POINT('Ctrl Pts',(104.958734125,1.25000000136558,-43.4753311640868));
#8558=CARTESIAN_POINT('Ctrl Pts',(104.958734125,1.18750000136558,-1.28537377788739E-14));
#8559=CARTESIAN_POINT('Ctrl Pts',(104.958734125,1.12500000136558,43.4753311640868));
#8560=CARTESIAN_POINT('Ctrl Pts',(74.2170326445434,1.06250000136558,74.2170326445434));
#8561=CARTESIAN_POINT('Ctrl Pts',(43.4753311640869,1.00000000136558,104.958734125));
#8562=CARTESIAN_POINT('Ctrl Pts',(1.92806066683109E-14,0.937500001365582,
104.958734125));
#8563=CARTESIAN_POINT('Ctrl Pts',(-43.4753311640868,0.875000001365582,104.958734125));
#8564=CARTESIAN_POINT('Ctrl Pts',(-74.2170326445434,0.812500001365582,74.2170326445434));
#8565=CARTESIAN_POINT('Ctrl Pts',(-104.958734125,0.750000001365582,43.4753311640869));
#8566=CARTESIAN_POINT('Ctrl Pts',(-104.958734125,0.687500001365582,0.));
#8567=CARTESIAN_POINT('Ctrl Pts',(-104.958734125,0.625000001365582,-43.4753311640868));
#8568=CARTESIAN_POINT('Ctrl Pts',(-74.2170326445434,0.562500001365582,-74.2170326445434));
#8569=CARTESIAN_POINT('Ctrl Pts',(-43.4753311640868,0.500000001365582,-104.958734125));
#8570=CARTESIAN_POINT('Ctrl Pts',(-6.42686888943697E-15,0.437500001365582,
-104.958734125));
#8571=CARTESIAN_POINT('Ctrl Pts',(43.4753311640868,0.375000001365582,-104.958734125));
#8572=CARTESIAN_POINT('Ctrl Pts',(74.2170326445434,0.312500001365582,-74.2170326445434));
#8573=CARTESIAN_POINT('Ctrl Pts',(104.958734125,0.250000001365581,-43.4753311640868));
#8574=CARTESIAN_POINT('Ctrl Pts',(104.958734125,0.187500001365581,-1.28537377788739E-14));
#8575=CARTESIAN_POINT('Ctrl Pts',(104.958734125,0.125000001365581,43.4753311640868));
#8576=CARTESIAN_POINT('Ctrl Pts',(74.2170326445434,0.0625000013655813,74.2170326445434));
#8577=CARTESIAN_POINT('Ctrl Pts',(43.4753311640869,1.36558125918285E-9,
104.958734125));
#8578=CARTESIAN_POINT('Ctrl Pts',(1.92806066683109E-14,-0.0624999986344188,
104.958734125));
#8579=CARTESIAN_POINT('Ctrl Pts',(-43.4753311640868,-0.124999998634419,
104.958734125));
#8580=CARTESIAN_POINT('Ctrl Pts',(-74.2170326445434,-0.187499998634419,
74.2170326445434));
#8581=CARTESIAN_POINT('Ctrl Pts',(-104.958734125,-0.249999998634419,43.4753311640869));
#8582=CARTESIAN_POINT('Ctrl Pts',(-104.958734125,-0.312499998634419,0.));
#8583=CARTESIAN_POINT('Ctrl Pts',(-105.5,50.,0.));
#8584=CARTESIAN_POINT('Ctrl Pts',(-105.5,49.9375,-43.6995308303615));
#8585=CARTESIAN_POINT('Ctrl Pts',(-74.5997654151808,49.875,-74.5997654151808));
#8586=CARTESIAN_POINT('Ctrl Pts',(-43.6995308303615,49.8125,-105.5));
#8587=CARTESIAN_POINT('Ctrl Pts',(-6.46001186550229E-15,49.75,-105.5));
#8588=CARTESIAN_POINT('Ctrl Pts',(43.6995308303615,49.6875,-105.5));
#8589=CARTESIAN_POINT('Ctrl Pts',(74.5997654151808,49.625,-74.5997654151808));
#8590=CARTESIAN_POINT('Ctrl Pts',(105.5,49.5625,-43.6995308303616));
#8591=CARTESIAN_POINT('Ctrl Pts',(105.5,49.5,-1.29200237310046E-14));
#8592=CARTESIAN_POINT('Ctrl Pts',(105.5,49.4375,43.6995308303615));
#8593=CARTESIAN_POINT('Ctrl Pts',(74.5997654151808,49.375,74.5997654151808));
#8594=CARTESIAN_POINT('Ctrl Pts',(43.6995308303616,49.3125,105.5));
#8595=CARTESIAN_POINT('Ctrl Pts',(1.93800355965069E-14,49.25,105.5));
#8596=CARTESIAN_POINT('Ctrl Pts',(-43.6995308303616,49.1875,105.5));
#8597=CARTESIAN_POINT('Ctrl Pts',(-74.5997654151808,49.125,74.5997654151808));
#8598=CARTESIAN_POINT('Ctrl Pts',(-105.5,49.0625,43.6995308303616));
#8599=CARTESIAN_POINT('Ctrl Pts',(-105.5,49.,0.));
#8600=CARTESIAN_POINT('Ctrl Pts',(-105.5,48.9375,-43.6995308303615));
#8601=CARTESIAN_POINT('Ctrl Pts',(-74.5997654151808,48.875,-74.5997654151808));
#8602=CARTESIAN_POINT('Ctrl Pts',(-43.6995308303615,48.8125,-105.5));
#8603=CARTESIAN_POINT('Ctrl Pts',(-6.46001186550229E-15,48.75,-105.5));
#8604=CARTESIAN_POINT('Ctrl Pts',(43.6995308303615,48.6875,-105.5));
#8605=CARTESIAN_POINT('Ctrl Pts',(74.5997654151808,48.625,-74.5997654151808));
#8606=CARTESIAN_POINT('Ctrl Pts',(105.5,48.5625,-43.6995308303616));
#8607=CARTESIAN_POINT('Ctrl Pts',(105.5,48.5,-1.29200237310046E-14));
#8608=CARTESIAN_POINT('Ctrl Pts',(105.5,48.4375,43.6995308303615));
#8609=CARTESIAN_POINT('Ctrl Pts',(74.5997654151808,48.375,74.5997654151808));
#8610=CARTESIAN_POINT('Ctrl Pts',(43.6995308303616,48.3125,105.5));
#8611=CARTESIAN_POINT('Ctrl Pts',(1.93800355965069E-14,48.25,105.5));
#8612=CARTESIAN_POINT('Ctrl Pts',(-43.6995308303616,48.1875,105.5));
#8613=CARTESIAN_POINT('Ctrl Pts',(-74.5997654151808,48.125,74.5997654151808));
#8614=CARTESIAN_POINT('Ctrl Pts',(-105.5,48.0625,43.6995308303616));
#8615=CARTESIAN_POINT('Ctrl Pts',(-105.5,48.,0.));
#8616=CARTESIAN_POINT('Ctrl Pts',(-105.5,47.9375,-43.6995308303615));
#8617=CARTESIAN_POINT('Ctrl Pts',(-74.5997654151808,47.875,-74.5997654151808));
#8618=CARTESIAN_POINT('Ctrl Pts',(-43.6995308303615,47.8125,-105.5));
#8619=CARTESIAN_POINT('Ctrl Pts',(-6.46001186550229E-15,47.75,-105.5));
#8620=CARTESIAN_POINT('Ctrl Pts',(43.6995308303615,47.6875,-105.5));
#8621=CARTESIAN_POINT('Ctrl Pts',(74.5997654151808,47.625,-74.5997654151808));
#8622=CARTESIAN_POINT('Ctrl Pts',(105.5,47.5625,-43.6995308303616));
#8623=CARTESIAN_POINT('Ctrl Pts',(105.5,47.5,-1.29200237310046E-14));
#8624=CARTESIAN_POINT('Ctrl Pts',(105.5,47.4375,43.6995308303615));
#8625=CARTESIAN_POINT('Ctrl Pts',(74.5997654151808,47.375,74.5997654151808));
#8626=CARTESIAN_POINT('Ctrl Pts',(43.6995308303616,47.3125,105.5));
#8627=CARTESIAN_POINT('Ctrl Pts',(1.93800355965069E-14,47.25,105.5));
#8628=CARTESIAN_POINT('Ctrl Pts',(-43.6995308303616,47.1875,105.5));
#8629=CARTESIAN_POINT('Ctrl Pts',(-74.5997654151808,47.125,74.5997654151808));
#8630=CARTESIAN_POINT('Ctrl Pts',(-105.5,47.0625,43.6995308303616));
#8631=CARTESIAN_POINT('Ctrl Pts',(-105.5,47.,0.));
#8632=CARTESIAN_POINT('Ctrl Pts',(-105.5,46.9375,-43.6995308303615));
#8633=CARTESIAN_POINT('Ctrl Pts',(-74.5997654151808,46.875,-74.5997654151808));
#8634=CARTESIAN_POINT('Ctrl Pts',(-43.6995308303615,46.8125,-105.5));
#8635=CARTESIAN_POINT('Ctrl Pts',(-6.46001186550229E-15,46.75,-105.5));
#8636=CARTESIAN_POINT('Ctrl Pts',(43.6995308303615,46.6875,-105.5));
#8637=CARTESIAN_POINT('Ctrl Pts',(74.5997654151808,46.625,-74.5997654151808));
#8638=CARTESIAN_POINT('Ctrl Pts',(105.5,46.5625,-43.6995308303616));
#8639=CARTESIAN_POINT('Ctrl Pts',(105.5,46.5,-1.29200237310046E-14));
#8640=CARTESIAN_POINT('Ctrl Pts',(105.5,46.4375,43.6995308303615));
#8641=CARTESIAN_POINT('Ctrl Pts',(74.5997654151808,46.375,74.5997654151808));
#8642=CARTESIAN_POINT('Ctrl Pts',(43.6995308303616,46.3125,105.5));
#8643=CARTESIAN_POINT('Ctrl Pts',(1.93800355965069E-14,46.25,105.5));
#8644=CARTESIAN_POINT('Ctrl Pts',(-43.6995308303616,46.1875,105.5));
#8645=CARTESIAN_POINT('Ctrl Pts',(-74.5997654151808,46.125,74.5997654151808));
#8646=CARTESIAN_POINT('Ctrl Pts',(-105.5,46.0625,43.6995308303616));
#8647=CARTESIAN_POINT('Ctrl Pts',(-105.5,46.,0.));
#8648=CARTESIAN_POINT('Ctrl Pts',(-105.5,45.9375,-43.6995308303615));
#8649=CARTESIAN_POINT('Ctrl Pts',(-74.5997654151808,45.875,-74.5997654151808));
#8650=CARTESIAN_POINT('Ctrl Pts',(-43.6995308303615,45.8125,-105.5));
#8651=CARTESIAN_POINT('Ctrl Pts',(-6.46001186550229E-15,45.75,-105.5));
#8652=CARTESIAN_POINT('Ctrl Pts',(43.6995308303615,45.6875,-105.5));
#8653=CARTESIAN_POINT('Ctrl Pts',(74.5997654151808,45.625,-74.5997654151808));
#8654=CARTESIAN_POINT('Ctrl Pts',(105.5,45.5625,-43.6995308303616));
#8655=CARTESIAN_POINT('Ctrl Pts',(105.5,45.5,-1.29200237310046E-14));
#8656=CARTESIAN_POINT('Ctrl Pts',(105.5,45.4375,43.6995308303615));
#8657=CARTESIAN_POINT('Ctrl Pts',(74.5997654151808,45.375,74.5997654151808));
#8658=CARTESIAN_POINT('Ctrl Pts',(43.6995308303616,45.3125,105.5));
#8659=CARTESIAN_POINT('Ctrl Pts',(1.93800355965069E-14,45.25,105.5));
#8660=CARTESIAN_POINT('Ctrl Pts',(-43.6995308303616,45.1875,105.5));
#8661=CARTESIAN_POINT('Ctrl Pts',(-74.5997654151808,45.125,74.5997654151808));
#8662=CARTESIAN_POINT('Ctrl Pts',(-105.5,45.0625,43.6995308303616));
#8663=CARTESIAN_POINT('Ctrl Pts',(-105.5,45.,0.));
#8664=CARTESIAN_POINT('Ctrl Pts',(-105.5,44.9375,-43.6995308303615));
#8665=CARTESIAN_POINT('Ctrl Pts',(-74.5997654151808,44.875,-74.5997654151808));
#8666=CARTESIAN_POINT('Ctrl Pts',(-43.6995308303615,44.8125,-105.5));
#8667=CARTESIAN_POINT('Ctrl Pts',(-6.46001186550229E-15,44.75,-105.5));
#8668=CARTESIAN_POINT('Ctrl Pts',(43.6995308303615,44.6875,-105.5));
#8669=CARTESIAN_POINT('Ctrl Pts',(74.5997654151808,44.625,-74.5997654151808));
#8670=CARTESIAN_POINT('Ctrl Pts',(105.5,44.5625,-43.6995308303616));
#8671=CARTESIAN_POINT('Ctrl Pts',(105.5,44.5,-1.29200237310046E-14));
#8672=CARTESIAN_POINT('Ctrl Pts',(105.5,44.4375,43.6995308303615));
#8673=CARTESIAN_POINT('Ctrl Pts',(74.5997654151808,44.375,74.5997654151808));
#8674=CARTESIAN_POINT('Ctrl Pts',(43.6995308303616,44.3125,105.5));
#8675=CARTESIAN_POINT('Ctrl Pts',(1.93800355965069E-14,44.25,105.5));
#8676=CARTESIAN_POINT('Ctrl Pts',(-43.6995308303616,44.1875,105.5));
#8677=CARTESIAN_POINT('Ctrl Pts',(-74.5997654151808,44.125,74.5997654151808));
#8678=CARTESIAN_POINT('Ctrl Pts',(-105.5,44.0625,43.6995308303616));
#8679=CARTESIAN_POINT('Ctrl Pts',(-105.5,44.,0.));
#8680=CARTESIAN_POINT('Ctrl Pts',(-105.5,43.9375,-43.6995308303615));
#8681=CARTESIAN_POINT('Ctrl Pts',(-74.5997654151808,43.875,-74.5997654151808));
#8682=CARTESIAN_POINT('Ctrl Pts',(-43.6995308303615,43.8125,-105.5));
#8683=CARTESIAN_POINT('Ctrl Pts',(-6.46001186550229E-15,43.75,-105.5));
#8684=CARTESIAN_POINT('Ctrl Pts',(43.6995308303615,43.6875,-105.5));
#8685=CARTESIAN_POINT('Ctrl Pts',(74.5997654151808,43.625,-74.5997654151808));
#8686=CARTESIAN_POINT('Ctrl Pts',(105.5,43.5625,-43.6995308303616));
#8687=CARTESIAN_POINT('Ctrl Pts',(105.5,43.5,-1.29200237310046E-14));
#8688=CARTESIAN_POINT('Ctrl Pts',(105.5,43.4375,43.6995308303615));
#8689=CARTESIAN_POINT('Ctrl Pts',(74.5997654151808,43.375,74.5997654151808));
#8690=CARTESIAN_POINT('Ctrl Pts',(43.6995308303616,43.3125,105.5));
#8691=CARTESIAN_POINT('Ctrl Pts',(1.93800355965069E-14,43.25,105.5));
#8692=CARTESIAN_POINT('Ctrl Pts',(-43.6995308303616,43.1875,105.5));
#8693=CARTESIAN_POINT('Ctrl Pts',(-74.5997654151808,43.125,74.5997654151808));
#8694=CARTESIAN_POINT('Ctrl Pts',(-105.5,43.0625,43.6995308303616));
#8695=CARTESIAN_POINT('Ctrl Pts',(-105.5,43.,0.));
#8696=CARTESIAN_POINT('Ctrl Pts',(-105.5,42.9375,-43.6995308303615));
#8697=CARTESIAN_POINT('Ctrl Pts',(-74.5997654151808,42.875,-74.5997654151808));
#8698=CARTESIAN_POINT('Ctrl Pts',(-43.6995308303615,42.8125,-105.5));
#8699=CARTESIAN_POINT('Ctrl Pts',(-6.46001186550229E-15,42.75,-105.5));
#8700=CARTESIAN_POINT('Ctrl Pts',(43.6995308303615,42.6875,-105.5));
#8701=CARTESIAN_POINT('Ctrl Pts',(74.5997654151808,42.625,-74.5997654151808));
#8702=CARTESIAN_POINT('Ctrl Pts',(105.5,42.5625,-43.6995308303616));
#8703=CARTESIAN_POINT('Ctrl Pts',(105.5,42.5,-1.29200237310046E-14));
#8704=CARTESIAN_POINT('Ctrl Pts',(105.5,42.4375,43.6995308303615));
#8705=CARTESIAN_POINT('Ctrl Pts',(74.5997654151808,42.375,74.5997654151808));
#8706=CARTESIAN_POINT('Ctrl Pts',(43.6995308303616,42.3125,105.5));
#8707=CARTESIAN_POINT('Ctrl Pts',(1.93800355965069E-14,42.25,105.5));
#8708=CARTESIAN_POINT('Ctrl Pts',(-43.6995308303616,42.1875,105.5));
#8709=CARTESIAN_POINT('Ctrl Pts',(-74.5997654151808,42.125,74.5997654151808));
#8710=CARTESIAN_POINT('Ctrl Pts',(-105.5,42.0625,43.6995308303616));
#8711=CARTESIAN_POINT('Ctrl Pts',(-105.5,42.,0.));
#8712=CARTESIAN_POINT('Ctrl Pts',(-105.5,41.9375,-43.6995308303615));
#8713=CARTESIAN_POINT('Ctrl Pts',(-74.5997654151808,41.875,-74.5997654151808));
#8714=CARTESIAN_POINT('Ctrl Pts',(-43.6995308303615,41.8125,-105.5));
#8715=CARTESIAN_POINT('Ctrl Pts',(-6.46001186550229E-15,41.75,-105.5));
#8716=CARTESIAN_POINT('Ctrl Pts',(43.6995308303615,41.6875,-105.5));
#8717=CARTESIAN_POINT('Ctrl Pts',(74.5997654151808,41.625,-74.5997654151808));
#8718=CARTESIAN_POINT('Ctrl Pts',(105.5,41.5625,-43.6995308303616));
#8719=CARTESIAN_POINT('Ctrl Pts',(105.5,41.5,-1.29200237310046E-14));
#8720=CARTESIAN_POINT('Ctrl Pts',(105.5,41.4375,43.6995308303615));
#8721=CARTESIAN_POINT('Ctrl Pts',(74.5997654151808,41.375,74.5997654151808));
#8722=CARTESIAN_POINT('Ctrl Pts',(43.6995308303616,41.3125,105.5));
#8723=CARTESIAN_POINT('Ctrl Pts',(1.93800355965069E-14,41.25,105.5));
#8724=CARTESIAN_POINT('Ctrl Pts',(-43.6995308303616,41.1875,105.5));
#8725=CARTESIAN_POINT('Ctrl Pts',(-74.5997654151808,41.125,74.5997654151808));
#8726=CARTESIAN_POINT('Ctrl Pts',(-105.5,41.0625,43.6995308303616));
#8727=CARTESIAN_POINT('Ctrl Pts',(-105.5,41.,0.));
#8728=CARTESIAN_POINT('Ctrl Pts',(-105.5,40.9375,-43.6995308303615));
#8729=CARTESIAN_POINT('Ctrl Pts',(-74.5997654151808,40.875,-74.5997654151808));
#8730=CARTESIAN_POINT('Ctrl Pts',(-43.6995308303615,40.8125,-105.5));
#8731=CARTESIAN_POINT('Ctrl Pts',(-6.46001186550229E-15,40.75,-105.5));
#8732=CARTESIAN_POINT('Ctrl Pts',(43.6995308303615,40.6875,-105.5));
#8733=CARTESIAN_POINT('Ctrl Pts',(74.5997654151808,40.625,-74.5997654151808));
#8734=CARTESIAN_POINT('Ctrl Pts',(105.5,40.5625,-43.6995308303616));
#8735=CARTESIAN_POINT('Ctrl Pts',(105.5,40.5,-1.29200237310046E-14));
#8736=CARTESIAN_POINT('Ctrl Pts',(105.5,40.4375,43.6995308303615));
#8737=CARTESIAN_POINT('Ctrl Pts',(74.5997654151808,40.375,74.5997654151808));
#8738=CARTESIAN_POINT('Ctrl Pts',(43.6995308303616,40.3125,105.5));
#8739=CARTESIAN_POINT('Ctrl Pts',(1.93800355965069E-14,40.25,105.5));
#8740=CARTESIAN_POINT('Ctrl Pts',(-43.6995308303616,40.1875,105.5));
#8741=CARTESIAN_POINT('Ctrl Pts',(-74.5997654151808,40.125,74.5997654151808));
#8742=CARTESIAN_POINT('Ctrl Pts',(-105.5,40.0625,43.6995308303616));
#8743=CARTESIAN_POINT('Ctrl Pts',(-105.5,40.,0.));
#8744=CARTESIAN_POINT('Ctrl Pts',(-105.5,39.9375,-43.6995308303615));
#8745=CARTESIAN_POINT('Ctrl Pts',(-74.5997654151808,39.875,-74.5997654151808));
#8746=CARTESIAN_POINT('Ctrl Pts',(-43.6995308303615,39.8125,-105.5));
#8747=CARTESIAN_POINT('Ctrl Pts',(-6.46001186550229E-15,39.75,-105.5));
#8748=CARTESIAN_POINT('Ctrl Pts',(43.6995308303615,39.6875,-105.5));
#8749=CARTESIAN_POINT('Ctrl Pts',(74.5997654151808,39.625,-74.5997654151808));
#8750=CARTESIAN_POINT('Ctrl Pts',(105.5,39.5625,-43.6995308303616));
#8751=CARTESIAN_POINT('Ctrl Pts',(105.5,39.5,-1.29200237310046E-14));
#8752=CARTESIAN_POINT('Ctrl Pts',(105.5,39.4375,43.6995308303615));
#8753=CARTESIAN_POINT('Ctrl Pts',(74.5997654151808,39.375,74.5997654151808));
#8754=CARTESIAN_POINT('Ctrl Pts',(43.6995308303616,39.3125,105.5));
#8755=CARTESIAN_POINT('Ctrl Pts',(1.93800355965069E-14,39.25,105.5));
#8756=CARTESIAN_POINT('Ctrl Pts',(-43.6995308303616,39.1875,105.5));
#8757=CARTESIAN_POINT('Ctrl Pts',(-74.5997654151808,39.125,74.5997654151808));
#8758=CARTESIAN_POINT('Ctrl Pts',(-105.5,39.0625,43.6995308303616));
#8759=CARTESIAN_POINT('Ctrl Pts',(-105.5,39.,0.));
#8760=CARTESIAN_POINT('Ctrl Pts',(-105.5,38.9375,-43.6995308303615));
#8761=CARTESIAN_POINT('Ctrl Pts',(-74.5997654151808,38.875,-74.5997654151808));
#8762=CARTESIAN_POINT('Ctrl Pts',(-43.6995308303615,38.8125,-105.5));
#8763=CARTESIAN_POINT('Ctrl Pts',(-6.46001186550229E-15,38.75,-105.5));
#8764=CARTESIAN_POINT('Ctrl Pts',(43.6995308303615,38.6875,-105.5));
#8765=CARTESIAN_POINT('Ctrl Pts',(74.5997654151808,38.625,-74.5997654151808));
#8766=CARTESIAN_POINT('Ctrl Pts',(105.5,38.5625,-43.6995308303616));
#8767=CARTESIAN_POINT('Ctrl Pts',(105.5,38.5,-1.29200237310046E-14));
#8768=CARTESIAN_POINT('Ctrl Pts',(105.5,38.4375,43.6995308303615));
#8769=CARTESIAN_POINT('Ctrl Pts',(74.5997654151808,38.375,74.5997654151808));
#8770=CARTESIAN_POINT('Ctrl Pts',(43.6995308303616,38.3125,105.5));
#8771=CARTESIAN_POINT('Ctrl Pts',(1.93800355965069E-14,38.25,105.5));
#8772=CARTESIAN_POINT('Ctrl Pts',(-43.6995308303616,38.1875,105.5));
#8773=CARTESIAN_POINT('Ctrl Pts',(-74.5997654151808,38.125,74.5997654151808));
#8774=CARTESIAN_POINT('Ctrl Pts',(-105.5,38.0625,43.6995308303616));
#8775=CARTESIAN_POINT('Ctrl Pts',(-105.5,38.,0.));
#8776=CARTESIAN_POINT('Ctrl Pts',(-105.5,37.9375,-43.6995308303615));
#8777=CARTESIAN_POINT('Ctrl Pts',(-74.5997654151808,37.875,-74.5997654151808));
#8778=CARTESIAN_POINT('Ctrl Pts',(-43.6995308303615,37.8125,-105.5));
#8779=CARTESIAN_POINT('Ctrl Pts',(-6.46001186550229E-15,37.75,-105.5));
#8780=CARTESIAN_POINT('Ctrl Pts',(43.6995308303615,37.6875,-105.5));
#8781=CARTESIAN_POINT('Ctrl Pts',(74.5997654151808,37.625,-74.5997654151808));
#8782=CARTESIAN_POINT('Ctrl Pts',(105.5,37.5625,-43.6995308303616));
#8783=CARTESIAN_POINT('Ctrl Pts',(105.5,37.5,-1.29200237310046E-14));
#8784=CARTESIAN_POINT('Ctrl Pts',(105.5,37.4375,43.6995308303615));
#8785=CARTESIAN_POINT('Ctrl Pts',(74.5997654151808,37.375,74.5997654151808));
#8786=CARTESIAN_POINT('Ctrl Pts',(43.6995308303616,37.3125,105.5));
#8787=CARTESIAN_POINT('Ctrl Pts',(1.93800355965069E-14,37.25,105.5));
#8788=CARTESIAN_POINT('Ctrl Pts',(-43.6995308303616,37.1875,105.5));
#8789=CARTESIAN_POINT('Ctrl Pts',(-74.5997654151808,37.125,74.5997654151808));
#8790=CARTESIAN_POINT('Ctrl Pts',(-105.5,37.0625,43.6995308303616));
#8791=CARTESIAN_POINT('Ctrl Pts',(-105.5,37.,0.));
#8792=CARTESIAN_POINT('Ctrl Pts',(-105.5,36.9375,-43.6995308303615));
#8793=CARTESIAN_POINT('Ctrl Pts',(-74.5997654151808,36.875,-74.5997654151808));
#8794=CARTESIAN_POINT('Ctrl Pts',(-43.6995308303615,36.8125,-105.5));
#8795=CARTESIAN_POINT('Ctrl Pts',(-6.46001186550229E-15,36.75,-105.5));
#8796=CARTESIAN_POINT('Ctrl Pts',(43.6995308303615,36.6875,-105.5));
#8797=CARTESIAN_POINT('Ctrl Pts',(74.5997654151808,36.625,-74.5997654151808));
#8798=CARTESIAN_POINT('Ctrl Pts',(105.5,36.5625,-43.6995308303616));
#8799=CARTESIAN_POINT('Ctrl Pts',(105.5,36.5,-1.29200237310046E-14));
#8800=CARTESIAN_POINT('Ctrl Pts',(105.5,36.4375,43.6995308303615));
#8801=CARTESIAN_POINT('Ctrl Pts',(74.5997654151808,36.375,74.5997654151808));
#8802=CARTESIAN_POINT('Ctrl Pts',(43.6995308303616,36.3125,105.5));
#8803=CARTESIAN_POINT('Ctrl Pts',(1.93800355965069E-14,36.25,105.5));
#8804=CARTESIAN_POINT('Ctrl Pts',(-43.6995308303616,36.1875,105.5));
#8805=CARTESIAN_POINT('Ctrl Pts',(-74.5997654151808,36.125,74.5997654151808));
#8806=CARTESIAN_POINT('Ctrl Pts',(-105.5,36.0625,43.6995308303616));
#8807=CARTESIAN_POINT('Ctrl Pts',(-105.5,36.,0.));
#8808=CARTESIAN_POINT('Ctrl Pts',(-105.5,35.9375,-43.6995308303615));
#8809=CARTESIAN_POINT('Ctrl Pts',(-74.5997654151808,35.875,-74.5997654151808));
#8810=CARTESIAN_POINT('Ctrl Pts',(-43.6995308303615,35.8125,-105.5));
#8811=CARTESIAN_POINT('Ctrl Pts',(-6.46001186550229E-15,35.75,-105.5));
#8812=CARTESIAN_POINT('Ctrl Pts',(43.6995308303615,35.6875,-105.5));
#8813=CARTESIAN_POINT('Ctrl Pts',(74.5997654151808,35.625,-74.5997654151808));
#8814=CARTESIAN_POINT('Ctrl Pts',(105.5,35.5625,-43.6995308303616));
#8815=CARTESIAN_POINT('Ctrl Pts',(105.5,35.5,-1.29200237310046E-14));
#8816=CARTESIAN_POINT('Ctrl Pts',(105.5,35.4375,43.6995308303615));
#8817=CARTESIAN_POINT('Ctrl Pts',(74.5997654151808,35.375,74.5997654151808));
#8818=CARTESIAN_POINT('Ctrl Pts',(43.6995308303616,35.3125,105.5));
#8819=CARTESIAN_POINT('Ctrl Pts',(1.93800355965069E-14,35.25,105.5));
#8820=CARTESIAN_POINT('Ctrl Pts',(-43.6995308303616,35.1875,105.5));
#8821=CARTESIAN_POINT('Ctrl Pts',(-74.5997654151808,35.125,74.5997654151808));
#8822=CARTESIAN_POINT('Ctrl Pts',(-105.5,35.0625,43.6995308303616));
#8823=CARTESIAN_POINT('Ctrl Pts',(-105.5,35.,0.));
#8824=CARTESIAN_POINT('Ctrl Pts',(-105.5,34.9375,-43.6995308303615));
#8825=CARTESIAN_POINT('Ctrl Pts',(-74.5997654151808,34.875,-74.5997654151808));
#8826=CARTESIAN_POINT('Ctrl Pts',(-43.6995308303615,34.8125,-105.5));
#8827=CARTESIAN_POINT('Ctrl Pts',(-6.46001186550229E-15,34.75,-105.5));
#8828=CARTESIAN_POINT('Ctrl Pts',(43.6995308303615,34.6875,-105.5));
#8829=CARTESIAN_POINT('Ctrl Pts',(74.5997654151808,34.625,-74.5997654151808));
#8830=CARTESIAN_POINT('Ctrl Pts',(105.5,34.5625,-43.6995308303616));
#8831=CARTESIAN_POINT('Ctrl Pts',(105.5,34.5,-1.29200237310046E-14));
#8832=CARTESIAN_POINT('Ctrl Pts',(105.5,34.4375,43.6995308303615));
#8833=CARTESIAN_POINT('Ctrl Pts',(74.5997654151808,34.375,74.5997654151808));
#8834=CARTESIAN_POINT('Ctrl Pts',(43.6995308303616,34.3125,105.5));
#8835=CARTESIAN_POINT('Ctrl Pts',(1.93800355965069E-14,34.25,105.5));
#8836=CARTESIAN_POINT('Ctrl Pts',(-43.6995308303616,34.1875,105.5));
#8837=CARTESIAN_POINT('Ctrl Pts',(-74.5997654151808,34.125,74.5997654151808));
#8838=CARTESIAN_POINT('Ctrl Pts',(-105.5,34.0625,43.6995308303616));
#8839=CARTESIAN_POINT('Ctrl Pts',(-105.5,34.,0.));
#8840=CARTESIAN_POINT('Ctrl Pts',(-105.5,33.9375,-43.6995308303615));
#8841=CARTESIAN_POINT('Ctrl Pts',(-74.5997654151808,33.875,-74.5997654151808));
#8842=CARTESIAN_POINT('Ctrl Pts',(-43.6995308303615,33.8125,-105.5));
#8843=CARTESIAN_POINT('Ctrl Pts',(-6.46001186550229E-15,33.75,-105.5));
#8844=CARTESIAN_POINT('Ctrl Pts',(43.6995308303615,33.6875,-105.5));
#8845=CARTESIAN_POINT('Ctrl Pts',(74.5997654151808,33.625,-74.5997654151808));
#8846=CARTESIAN_POINT('Ctrl Pts',(105.5,33.5625,-43.6995308303616));
#8847=CARTESIAN_POINT('Ctrl Pts',(105.5,33.5,-1.29200237310046E-14));
#8848=CARTESIAN_POINT('Ctrl Pts',(105.5,33.4375,43.6995308303615));
#8849=CARTESIAN_POINT('Ctrl Pts',(74.5997654151808,33.375,74.5997654151808));
#8850=CARTESIAN_POINT('Ctrl Pts',(43.6995308303616,33.3125,105.5));
#8851=CARTESIAN_POINT('Ctrl Pts',(1.93800355965069E-14,33.25,105.5));
#8852=CARTESIAN_POINT('Ctrl Pts',(-43.6995308303616,33.1875,105.5));
#8853=CARTESIAN_POINT('Ctrl Pts',(-74.5997654151808,33.125,74.5997654151808));
#8854=CARTESIAN_POINT('Ctrl Pts',(-105.5,33.0625,43.6995308303616));
#8855=CARTESIAN_POINT('Ctrl Pts',(-105.5,33.,0.));
#8856=CARTESIAN_POINT('Ctrl Pts',(-105.5,32.9375,-43.6995308303615));
#8857=CARTESIAN_POINT('Ctrl Pts',(-74.5997654151808,32.875,-74.5997654151808));
#8858=CARTESIAN_POINT('Ctrl Pts',(-43.6995308303615,32.8125,-105.5));
#8859=CARTESIAN_POINT('Ctrl Pts',(-6.46001186550229E-15,32.75,-105.5));
#8860=CARTESIAN_POINT('Ctrl Pts',(43.6995308303615,32.6875,-105.5));
#8861=CARTESIAN_POINT('Ctrl Pts',(74.5997654151808,32.625,-74.5997654151808));
#8862=CARTESIAN_POINT('Ctrl Pts',(105.5,32.5625,-43.6995308303616));
#8863=CARTESIAN_POINT('Ctrl Pts',(105.5,32.5,-1.29200237310046E-14));
#8864=CARTESIAN_POINT('Ctrl Pts',(105.5,32.4375,43.6995308303615));
#8865=CARTESIAN_POINT('Ctrl Pts',(74.5997654151808,32.375,74.5997654151808));
#8866=CARTESIAN_POINT('Ctrl Pts',(43.6995308303616,32.3125,105.5));
#8867=CARTESIAN_POINT('Ctrl Pts',(1.93800355965069E-14,32.25,105.5));
#8868=CARTESIAN_POINT('Ctrl Pts',(-43.6995308303616,32.1875,105.5));
#8869=CARTESIAN_POINT('Ctrl Pts',(-74.5997654151808,32.125,74.5997654151808));
#8870=CARTESIAN_POINT('Ctrl Pts',(-105.5,32.0625,43.6995308303616));
#8871=CARTESIAN_POINT('Ctrl Pts',(-105.5,32.,0.));
#8872=CARTESIAN_POINT('Ctrl Pts',(-105.5,31.9375,-43.6995308303615));
#8873=CARTESIAN_POINT('Ctrl Pts',(-74.5997654151808,31.875,-74.5997654151808));
#8874=CARTESIAN_POINT('Ctrl Pts',(-43.6995308303615,31.8125,-105.5));
#8875=CARTESIAN_POINT('Ctrl Pts',(-6.46001186550229E-15,31.75,-105.5));
#8876=CARTESIAN_POINT('Ctrl Pts',(43.6995308303615,31.6875,-105.5));
#8877=CARTESIAN_POINT('Ctrl Pts',(74.5997654151808,31.625,-74.5997654151808));
#8878=CARTESIAN_POINT('Ctrl Pts',(105.5,31.5625,-43.6995308303616));
#8879=CARTESIAN_POINT('Ctrl Pts',(105.5,31.5,-1.29200237310046E-14));
#8880=CARTESIAN_POINT('Ctrl Pts',(105.5,31.4375,43.6995308303615));
#8881=CARTESIAN_POINT('Ctrl Pts',(74.5997654151808,31.375,74.5997654151808));
#8882=CARTESIAN_POINT('Ctrl Pts',(43.6995308303616,31.3125,105.5));
#8883=CARTESIAN_POINT('Ctrl Pts',(1.93800355965069E-14,31.25,105.5));
#8884=CARTESIAN_POINT('Ctrl Pts',(-43.6995308303616,31.1875,105.5));
#8885=CARTESIAN_POINT('Ctrl Pts',(-74.5997654151808,31.125,74.5997654151808));
#8886=CARTESIAN_POINT('Ctrl Pts',(-105.5,31.0625,43.6995308303616));
#8887=CARTESIAN_POINT('Ctrl Pts',(-105.5,31.,0.));
#8888=CARTESIAN_POINT('Ctrl Pts',(-105.5,30.9375,-43.6995308303615));
#8889=CARTESIAN_POINT('Ctrl Pts',(-74.5997654151808,30.875,-74.5997654151808));
#8890=CARTESIAN_POINT('Ctrl Pts',(-43.6995308303615,30.8125,-105.5));
#8891=CARTESIAN_POINT('Ctrl Pts',(-6.46001186550229E-15,30.75,-105.5));
#8892=CARTESIAN_POINT('Ctrl Pts',(43.6995308303615,30.6875,-105.5));
#8893=CARTESIAN_POINT('Ctrl Pts',(74.5997654151808,30.625,-74.5997654151808));
#8894=CARTESIAN_POINT('Ctrl Pts',(105.5,30.5625,-43.6995308303616));
#8895=CARTESIAN_POINT('Ctrl Pts',(105.5,30.5,-1.29200237310046E-14));
#8896=CARTESIAN_POINT('Ctrl Pts',(105.5,30.4375,43.6995308303615));
#8897=CARTESIAN_POINT('Ctrl Pts',(74.5997654151808,30.375,74.5997654151808));
#8898=CARTESIAN_POINT('Ctrl Pts',(43.6995308303616,30.3125,105.5));
#8899=CARTESIAN_POINT('Ctrl Pts',(1.93800355965069E-14,30.25,105.5));
#8900=CARTESIAN_POINT('Ctrl Pts',(-43.6995308303616,30.1875,105.5));
#8901=CARTESIAN_POINT('Ctrl Pts',(-74.5997654151808,30.125,74.5997654151808));
#8902=CARTESIAN_POINT('Ctrl Pts',(-105.5,30.0625,43.6995308303616));
#8903=CARTESIAN_POINT('Ctrl Pts',(-105.5,30.,0.));
#8904=CARTESIAN_POINT('Ctrl Pts',(-105.5,29.9375,-43.6995308303615));
#8905=CARTESIAN_POINT('Ctrl Pts',(-74.5997654151808,29.875,-74.5997654151808));
#8906=CARTESIAN_POINT('Ctrl Pts',(-43.6995308303615,29.8125,-105.5));
#8907=CARTESIAN_POINT('Ctrl Pts',(-6.46001186550229E-15,29.75,-105.5));
#8908=CARTESIAN_POINT('Ctrl Pts',(43.6995308303615,29.6875,-105.5));
#8909=CARTESIAN_POINT('Ctrl Pts',(74.5997654151808,29.625,-74.5997654151808));
#8910=CARTESIAN_POINT('Ctrl Pts',(105.5,29.5625,-43.6995308303616));
#8911=CARTESIAN_POINT('Ctrl Pts',(105.5,29.5,-1.29200237310046E-14));
#8912=CARTESIAN_POINT('Ctrl Pts',(105.5,29.4375,43.6995308303615));
#8913=CARTESIAN_POINT('Ctrl Pts',(74.5997654151808,29.375,74.5997654151808));
#8914=CARTESIAN_POINT('Ctrl Pts',(43.6995308303616,29.3125,105.5));
#8915=CARTESIAN_POINT('Ctrl Pts',(1.93800355965069E-14,29.25,105.5));
#8916=CARTESIAN_POINT('Ctrl Pts',(-43.6995308303616,29.1875,105.5));
#8917=CARTESIAN_POINT('Ctrl Pts',(-74.5997654151808,29.125,74.5997654151808));
#8918=CARTESIAN_POINT('Ctrl Pts',(-105.5,29.0625,43.6995308303616));
#8919=CARTESIAN_POINT('Ctrl Pts',(-105.5,29.,0.));
#8920=CARTESIAN_POINT('Ctrl Pts',(-105.5,28.9375,-43.6995308303615));
#8921=CARTESIAN_POINT('Ctrl Pts',(-74.5997654151808,28.875,-74.5997654151808));
#8922=CARTESIAN_POINT('Ctrl Pts',(-43.6995308303615,28.8125,-105.5));
#8923=CARTESIAN_POINT('Ctrl Pts',(-6.46001186550229E-15,28.75,-105.5));
#8924=CARTESIAN_POINT('Ctrl Pts',(43.6995308303615,28.6875,-105.5));
#8925=CARTESIAN_POINT('Ctrl Pts',(74.5997654151808,28.625,-74.5997654151808));
#8926=CARTESIAN_POINT('Ctrl Pts',(105.5,28.5625,-43.6995308303616));
#8927=CARTESIAN_POINT('Ctrl Pts',(105.5,28.5,-1.29200237310046E-14));
#8928=CARTESIAN_POINT('Ctrl Pts',(105.5,28.4375,43.6995308303615));
#8929=CARTESIAN_POINT('Ctrl Pts',(74.5997654151808,28.375,74.5997654151808));
#8930=CARTESIAN_POINT('Ctrl Pts',(43.6995308303616,28.3125,105.5));
#8931=CARTESIAN_POINT('Ctrl Pts',(1.93800355965069E-14,28.25,105.5));
#8932=CARTESIAN_POINT('Ctrl Pts',(-43.6995308303616,28.1875,105.5));
#8933=CARTESIAN_POINT('Ctrl Pts',(-74.5997654151808,28.125,74.5997654151808));
#8934=CARTESIAN_POINT('Ctrl Pts',(-105.5,28.0625,43.6995308303616));
#8935=CARTESIAN_POINT('Ctrl Pts',(-105.5,28.,0.));
#8936=CARTESIAN_POINT('Ctrl Pts',(-105.5,27.9375,-43.6995308303615));
#8937=CARTESIAN_POINT('Ctrl Pts',(-74.5997654151808,27.875,-74.5997654151808));
#8938=CARTESIAN_POINT('Ctrl Pts',(-43.6995308303615,27.8125,-105.5));
#8939=CARTESIAN_POINT('Ctrl Pts',(-6.46001186550229E-15,27.75,-105.5));
#8940=CARTESIAN_POINT('Ctrl Pts',(43.6995308303615,27.6875,-105.5));
#8941=CARTESIAN_POINT('Ctrl Pts',(74.5997654151808,27.625,-74.5997654151808));
#8942=CARTESIAN_POINT('Ctrl Pts',(105.5,27.5625,-43.6995308303616));
#8943=CARTESIAN_POINT('Ctrl Pts',(105.5,27.5,-1.29200237310046E-14));
#8944=CARTESIAN_POINT('Ctrl Pts',(105.5,27.4375,43.6995308303615));
#8945=CARTESIAN_POINT('Ctrl Pts',(74.5997654151808,27.375,74.5997654151808));
#8946=CARTESIAN_POINT('Ctrl Pts',(43.6995308303616,27.3125,105.5));
#8947=CARTESIAN_POINT('Ctrl Pts',(1.93800355965069E-14,27.25,105.5));
#8948=CARTESIAN_POINT('Ctrl Pts',(-43.6995308303616,27.1875,105.5));
#8949=CARTESIAN_POINT('Ctrl Pts',(-74.5997654151808,27.125,74.5997654151808));
#8950=CARTESIAN_POINT('Ctrl Pts',(-105.5,27.0625,43.6995308303616));
#8951=CARTESIAN_POINT('Ctrl Pts',(-105.5,27.,0.));
#8952=CARTESIAN_POINT('Ctrl Pts',(-105.5,26.9375,-43.6995308303615));
#8953=CARTESIAN_POINT('Ctrl Pts',(-74.5997654151808,26.875,-74.5997654151808));
#8954=CARTESIAN_POINT('Ctrl Pts',(-43.6995308303615,26.8125,-105.5));
#8955=CARTESIAN_POINT('Ctrl Pts',(-6.46001186550229E-15,26.75,-105.5));
#8956=CARTESIAN_POINT('Ctrl Pts',(43.6995308303615,26.6875,-105.5));
#8957=CARTESIAN_POINT('Ctrl Pts',(74.5997654151808,26.625,-74.5997654151808));
#8958=CARTESIAN_POINT('Ctrl Pts',(105.5,26.5625,-43.6995308303616));
#8959=CARTESIAN_POINT('Ctrl Pts',(105.5,26.5,-1.29200237310046E-14));
#8960=CARTESIAN_POINT('Ctrl Pts',(105.5,26.4375,43.6995308303615));
#8961=CARTESIAN_POINT('Ctrl Pts',(74.5997654151808,26.375,74.5997654151808));
#8962=CARTESIAN_POINT('Ctrl Pts',(43.6995308303616,26.3125,105.5));
#8963=CARTESIAN_POINT('Ctrl Pts',(1.93800355965069E-14,26.25,105.5));
#8964=CARTESIAN_POINT('Ctrl Pts',(-43.6995308303616,26.1875,105.5));
#8965=CARTESIAN_POINT('Ctrl Pts',(-74.5997654151808,26.125,74.5997654151808));
#8966=CARTESIAN_POINT('Ctrl Pts',(-105.5,26.0625,43.6995308303616));
#8967=CARTESIAN_POINT('Ctrl Pts',(-105.5,26.,0.));
#8968=CARTESIAN_POINT('Ctrl Pts',(-105.5,25.9375,-43.6995308303615));
#8969=CARTESIAN_POINT('Ctrl Pts',(-74.5997654151808,25.875,-74.5997654151808));
#8970=CARTESIAN_POINT('Ctrl Pts',(-43.6995308303615,25.8125,-105.5));
#8971=CARTESIAN_POINT('Ctrl Pts',(-6.46001186550229E-15,25.75,-105.5));
#8972=CARTESIAN_POINT('Ctrl Pts',(43.6995308303615,25.6875,-105.5));
#8973=CARTESIAN_POINT('Ctrl Pts',(74.5997654151808,25.625,-74.5997654151808));
#8974=CARTESIAN_POINT('Ctrl Pts',(105.5,25.5625,-43.6995308303616));
#8975=CARTESIAN_POINT('Ctrl Pts',(105.5,25.5,-1.29200237310046E-14));
#8976=CARTESIAN_POINT('Ctrl Pts',(105.5,25.4375,43.6995308303615));
#8977=CARTESIAN_POINT('Ctrl Pts',(74.5997654151808,25.375,74.5997654151808));
#8978=CARTESIAN_POINT('Ctrl Pts',(43.6995308303616,25.3125,105.5));
#8979=CARTESIAN_POINT('Ctrl Pts',(1.93800355965069E-14,25.25,105.5));
#8980=CARTESIAN_POINT('Ctrl Pts',(-43.6995308303616,25.1875,105.5));
#8981=CARTESIAN_POINT('Ctrl Pts',(-74.5997654151808,25.125,74.5997654151808));
#8982=CARTESIAN_POINT('Ctrl Pts',(-105.5,25.0625,43.6995308303616));
#8983=CARTESIAN_POINT('Ctrl Pts',(-105.5,25.,0.));
#8984=CARTESIAN_POINT('Ctrl Pts',(-105.5,24.9375,-43.6995308303615));
#8985=CARTESIAN_POINT('Ctrl Pts',(-74.5997654151808,24.875,-74.5997654151808));
#8986=CARTESIAN_POINT('Ctrl Pts',(-43.6995308303615,24.8125,-105.5));
#8987=CARTESIAN_POINT('Ctrl Pts',(-6.46001186550229E-15,24.75,-105.5));
#8988=CARTESIAN_POINT('Ctrl Pts',(43.6995308303615,24.6875,-105.5));
#8989=CARTESIAN_POINT('Ctrl Pts',(74.5997654151808,24.625,-74.5997654151808));
#8990=CARTESIAN_POINT('Ctrl Pts',(105.5,24.5625,-43.6995308303616));
#8991=CARTESIAN_POINT('Ctrl Pts',(105.5,24.5,-1.29200237310046E-14));
#8992=CARTESIAN_POINT('Ctrl Pts',(105.5,24.4375,43.6995308303615));
#8993=CARTESIAN_POINT('Ctrl Pts',(74.5997654151808,24.375,74.5997654151808));
#8994=CARTESIAN_POINT('Ctrl Pts',(43.6995308303616,24.3125,105.5));
#8995=CARTESIAN_POINT('Ctrl Pts',(1.93800355965069E-14,24.25,105.5));
#8996=CARTESIAN_POINT('Ctrl Pts',(-43.6995308303616,24.1875,105.5));
#8997=CARTESIAN_POINT('Ctrl Pts',(-74.5997654151808,24.125,74.5997654151808));
#8998=CARTESIAN_POINT('Ctrl Pts',(-105.5,24.0625,43.6995308303616));
#8999=CARTESIAN_POINT('Ctrl Pts',(-105.5,24.,0.));
#9000=CARTESIAN_POINT('Ctrl Pts',(-105.5,23.9375,-43.6995308303615));
#9001=CARTESIAN_POINT('Ctrl Pts',(-74.5997654151808,23.875,-74.5997654151808));
#9002=CARTESIAN_POINT('Ctrl Pts',(-43.6995308303615,23.8125,-105.5));
#9003=CARTESIAN_POINT('Ctrl Pts',(-6.46001186550229E-15,23.75,-105.5));
#9004=CARTESIAN_POINT('Ctrl Pts',(43.6995308303615,23.6875,-105.5));
#9005=CARTESIAN_POINT('Ctrl Pts',(74.5997654151808,23.625,-74.5997654151808));
#9006=CARTESIAN_POINT('Ctrl Pts',(105.5,23.5625,-43.6995308303616));
#9007=CARTESIAN_POINT('Ctrl Pts',(105.5,23.5,-1.29200237310046E-14));
#9008=CARTESIAN_POINT('Ctrl Pts',(105.5,23.4375,43.6995308303615));
#9009=CARTESIAN_POINT('Ctrl Pts',(74.5997654151808,23.375,74.5997654151808));
#9010=CARTESIAN_POINT('Ctrl Pts',(43.6995308303616,23.3125,105.5));
#9011=CARTESIAN_POINT('Ctrl Pts',(1.93800355965069E-14,23.25,105.5));
#9012=CARTESIAN_POINT('Ctrl Pts',(-43.6995308303616,23.1875,105.5));
#9013=CARTESIAN_POINT('Ctrl Pts',(-74.5997654151808,23.125,74.5997654151808));
#9014=CARTESIAN_POINT('Ctrl Pts',(-105.5,23.0625,43.6995308303616));
#9015=CARTESIAN_POINT('Ctrl Pts',(-105.5,23.,0.));
#9016=CARTESIAN_POINT('Ctrl Pts',(-105.5,22.9375,-43.6995308303615));
#9017=CARTESIAN_POINT('Ctrl Pts',(-74.5997654151808,22.875,-74.5997654151808));
#9018=CARTESIAN_POINT('Ctrl Pts',(-43.6995308303615,22.8125,-105.5));
#9019=CARTESIAN_POINT('Ctrl Pts',(-6.46001186550229E-15,22.75,-105.5));
#9020=CARTESIAN_POINT('Ctrl Pts',(43.6995308303615,22.6875,-105.5));
#9021=CARTESIAN_POINT('Ctrl Pts',(74.5997654151808,22.625,-74.5997654151808));
#9022=CARTESIAN_POINT('Ctrl Pts',(105.5,22.5625,-43.6995308303616));
#9023=CARTESIAN_POINT('Ctrl Pts',(105.5,22.5,-1.29200237310046E-14));
#9024=CARTESIAN_POINT('Ctrl Pts',(105.5,22.4375,43.6995308303615));
#9025=CARTESIAN_POINT('Ctrl Pts',(74.5997654151808,22.375,74.5997654151808));
#9026=CARTESIAN_POINT('Ctrl Pts',(43.6995308303616,22.3125,105.5));
#9027=CARTESIAN_POINT('Ctrl Pts',(1.93800355965069E-14,22.25,105.5));
#9028=CARTESIAN_POINT('Ctrl Pts',(-43.6995308303616,22.1875,105.5));
#9029=CARTESIAN_POINT('Ctrl Pts',(-74.5997654151808,22.125,74.5997654151808));
#9030=CARTESIAN_POINT('Ctrl Pts',(-105.5,22.0625,43.6995308303616));
#9031=CARTESIAN_POINT('Ctrl Pts',(-105.5,22.,0.));
#9032=CARTESIAN_POINT('Ctrl Pts',(-105.5,21.9375,-43.6995308303615));
#9033=CARTESIAN_POINT('Ctrl Pts',(-74.5997654151808,21.875,-74.5997654151808));
#9034=CARTESIAN_POINT('Ctrl Pts',(-43.6995308303615,21.8125,-105.5));
#9035=CARTESIAN_POINT('Ctrl Pts',(-6.46001186550229E-15,21.75,-105.5));
#9036=CARTESIAN_POINT('Ctrl Pts',(43.6995308303615,21.6875,-105.5));
#9037=CARTESIAN_POINT('Ctrl Pts',(74.5997654151808,21.625,-74.5997654151808));
#9038=CARTESIAN_POINT('Ctrl Pts',(105.5,21.5625,-43.6995308303616));
#9039=CARTESIAN_POINT('Ctrl Pts',(105.5,21.5,-1.29200237310046E-14));
#9040=CARTESIAN_POINT('Ctrl Pts',(105.5,21.4375,43.6995308303615));
#9041=CARTESIAN_POINT('Ctrl Pts',(74.5997654151808,21.375,74.5997654151808));
#9042=CARTESIAN_POINT('Ctrl Pts',(43.6995308303616,21.3125,105.5));
#9043=CARTESIAN_POINT('Ctrl Pts',(1.93800355965069E-14,21.25,105.5));
#9044=CARTESIAN_POINT('Ctrl Pts',(-43.6995308303616,21.1875,105.5));
#9045=CARTESIAN_POINT('Ctrl Pts',(-74.5997654151808,21.125,74.5997654151808));
#9046=CARTESIAN_POINT('Ctrl Pts',(-105.5,21.0625,43.6995308303616));
#9047=CARTESIAN_POINT('Ctrl Pts',(-105.5,21.,0.));
#9048=CARTESIAN_POINT('Ctrl Pts',(-105.5,20.9375,-43.6995308303615));
#9049=CARTESIAN_POINT('Ctrl Pts',(-74.5997654151808,20.875,-74.5997654151808));
#9050=CARTESIAN_POINT('Ctrl Pts',(-43.6995308303615,20.8125,-105.5));
#9051=CARTESIAN_POINT('Ctrl Pts',(-6.46001186550229E-15,20.75,-105.5));
#9052=CARTESIAN_POINT('Ctrl Pts',(43.6995308303615,20.6875,-105.5));
#9053=CARTESIAN_POINT('Ctrl Pts',(74.5997654151808,20.625,-74.5997654151808));
#9054=CARTESIAN_POINT('Ctrl Pts',(105.5,20.5625,-43.6995308303616));
#9055=CARTESIAN_POINT('Ctrl Pts',(105.5,20.5,-1.29200237310046E-14));
#9056=CARTESIAN_POINT('Ctrl Pts',(105.5,20.4375,43.6995308303615));
#9057=CARTESIAN_POINT('Ctrl Pts',(74.5997654151808,20.375,74.5997654151808));
#9058=CARTESIAN_POINT('Ctrl Pts',(43.6995308303616,20.3125,105.5));
#9059=CARTESIAN_POINT('Ctrl Pts',(1.93800355965069E-14,20.25,105.5));
#9060=CARTESIAN_POINT('Ctrl Pts',(-43.6995308303616,20.1875,105.5));
#9061=CARTESIAN_POINT('Ctrl Pts',(-74.5997654151808,20.125,74.5997654151808));
#9062=CARTESIAN_POINT('Ctrl Pts',(-105.5,20.0625,43.6995308303616));
#9063=CARTESIAN_POINT('Ctrl Pts',(-105.5,20.,0.));
#9064=CARTESIAN_POINT('Ctrl Pts',(-105.5,19.9375,-43.6995308303615));
#9065=CARTESIAN_POINT('Ctrl Pts',(-74.5997654151808,19.875,-74.5997654151808));
#9066=CARTESIAN_POINT('Ctrl Pts',(-43.6995308303615,19.8125,-105.5));
#9067=CARTESIAN_POINT('Ctrl Pts',(-6.46001186550229E-15,19.75,-105.5));
#9068=CARTESIAN_POINT('Ctrl Pts',(43.6995308303615,19.6875,-105.5));
#9069=CARTESIAN_POINT('Ctrl Pts',(74.5997654151808,19.625,-74.5997654151808));
#9070=CARTESIAN_POINT('Ctrl Pts',(105.5,19.5625,-43.6995308303616));
#9071=CARTESIAN_POINT('Ctrl Pts',(105.5,19.5,-1.29200237310046E-14));
#9072=CARTESIAN_POINT('Ctrl Pts',(105.5,19.4375,43.6995308303615));
#9073=CARTESIAN_POINT('Ctrl Pts',(74.5997654151808,19.375,74.5997654151808));
#9074=CARTESIAN_POINT('Ctrl Pts',(43.6995308303616,19.3125,105.5));
#9075=CARTESIAN_POINT('Ctrl Pts',(1.93800355965069E-14,19.25,105.5));
#9076=CARTESIAN_POINT('Ctrl Pts',(-43.6995308303616,19.1875,105.5));
#9077=CARTESIAN_POINT('Ctrl Pts',(-74.5997654151808,19.125,74.5997654151808));
#9078=CARTESIAN_POINT('Ctrl Pts',(-105.5,19.0625,43.6995308303616));
#9079=CARTESIAN_POINT('Ctrl Pts',(-105.5,19.,0.));
#9080=CARTESIAN_POINT('Ctrl Pts',(-105.5,18.9375,-43.6995308303615));
#9081=CARTESIAN_POINT('Ctrl Pts',(-74.5997654151808,18.875,-74.5997654151808));
#9082=CARTESIAN_POINT('Ctrl Pts',(-43.6995308303615,18.8125,-105.5));
#9083=CARTESIAN_POINT('Ctrl Pts',(-6.46001186550229E-15,18.75,-105.5));
#9084=CARTESIAN_POINT('Ctrl Pts',(43.6995308303615,18.6875,-105.5));
#9085=CARTESIAN_POINT('Ctrl Pts',(74.5997654151808,18.625,-74.5997654151808));
#9086=CARTESIAN_POINT('Ctrl Pts',(105.5,18.5625,-43.6995308303616));
#9087=CARTESIAN_POINT('Ctrl Pts',(105.5,18.5,-1.29200237310046E-14));
#9088=CARTESIAN_POINT('Ctrl Pts',(105.5,18.4375,43.6995308303615));
#9089=CARTESIAN_POINT('Ctrl Pts',(74.5997654151808,18.375,74.5997654151808));
#9090=CARTESIAN_POINT('Ctrl Pts',(43.6995308303616,18.3125,105.5));
#9091=CARTESIAN_POINT('Ctrl Pts',(1.93800355965069E-14,18.25,105.5));
#9092=CARTESIAN_POINT('Ctrl Pts',(-43.6995308303616,18.1875,105.5));
#9093=CARTESIAN_POINT('Ctrl Pts',(-74.5997654151808,18.125,74.5997654151808));
#9094=CARTESIAN_POINT('Ctrl Pts',(-105.5,18.0625,43.6995308303616));
#9095=CARTESIAN_POINT('Ctrl Pts',(-105.5,18.,0.));
#9096=CARTESIAN_POINT('Ctrl Pts',(-105.5,17.9375,-43.6995308303615));
#9097=CARTESIAN_POINT('Ctrl Pts',(-74.5997654151808,17.875,-74.5997654151808));
#9098=CARTESIAN_POINT('Ctrl Pts',(-43.6995308303615,17.8125,-105.5));
#9099=CARTESIAN_POINT('Ctrl Pts',(-6.46001186550229E-15,17.75,-105.5));
#9100=CARTESIAN_POINT('Ctrl Pts',(43.6995308303615,17.6875,-105.5));
#9101=CARTESIAN_POINT('Ctrl Pts',(74.5997654151808,17.625,-74.5997654151808));
#9102=CARTESIAN_POINT('Ctrl Pts',(105.5,17.5625,-43.6995308303616));
#9103=CARTESIAN_POINT('Ctrl Pts',(105.5,17.5,-1.29200237310046E-14));
#9104=CARTESIAN_POINT('Ctrl Pts',(105.5,17.4375,43.6995308303615));
#9105=CARTESIAN_POINT('Ctrl Pts',(74.5997654151808,17.375,74.5997654151808));
#9106=CARTESIAN_POINT('Ctrl Pts',(43.6995308303616,17.3125,105.5));
#9107=CARTESIAN_POINT('Ctrl Pts',(1.93800355965069E-14,17.25,105.5));
#9108=CARTESIAN_POINT('Ctrl Pts',(-43.6995308303616,17.1875,105.5));
#9109=CARTESIAN_POINT('Ctrl Pts',(-74.5997654151808,17.125,74.5997654151808));
#9110=CARTESIAN_POINT('Ctrl Pts',(-105.5,17.0625,43.6995308303616));
#9111=CARTESIAN_POINT('Ctrl Pts',(-105.5,17.,0.));
#9112=CARTESIAN_POINT('Ctrl Pts',(-105.5,16.9375,-43.6995308303615));
#9113=CARTESIAN_POINT('Ctrl Pts',(-74.5997654151808,16.875,-74.5997654151808));
#9114=CARTESIAN_POINT('Ctrl Pts',(-43.6995308303615,16.8125,-105.5));
#9115=CARTESIAN_POINT('Ctrl Pts',(-6.46001186550229E-15,16.75,-105.5));
#9116=CARTESIAN_POINT('Ctrl Pts',(43.6995308303615,16.6875,-105.5));
#9117=CARTESIAN_POINT('Ctrl Pts',(74.5997654151808,16.625,-74.5997654151808));
#9118=CARTESIAN_POINT('Ctrl Pts',(105.5,16.5625,-43.6995308303616));
#9119=CARTESIAN_POINT('Ctrl Pts',(105.5,16.5,-1.29200237310046E-14));
#9120=CARTESIAN_POINT('Ctrl Pts',(105.5,16.4375,43.6995308303615));
#9121=CARTESIAN_POINT('Ctrl Pts',(74.5997654151808,16.375,74.5997654151808));
#9122=CARTESIAN_POINT('Ctrl Pts',(43.6995308303616,16.3125,105.5));
#9123=CARTESIAN_POINT('Ctrl Pts',(1.93800355965069E-14,16.25,105.5));
#9124=CARTESIAN_POINT('Ctrl Pts',(-43.6995308303616,16.1875,105.5));
#9125=CARTESIAN_POINT('Ctrl Pts',(-74.5997654151808,16.125,74.5997654151808));
#9126=CARTESIAN_POINT('Ctrl Pts',(-105.5,16.0625,43.6995308303616));
#9127=CARTESIAN_POINT('Ctrl Pts',(-105.5,16.,0.));
#9128=CARTESIAN_POINT('Ctrl Pts',(-105.5,15.9375,-43.6995308303615));
#9129=CARTESIAN_POINT('Ctrl Pts',(-74.5997654151808,15.875,-74.5997654151808));
#9130=CARTESIAN_POINT('Ctrl Pts',(-43.6995308303615,15.8125,-105.5));
#9131=CARTESIAN_POINT('Ctrl Pts',(-6.46001186550229E-15,15.75,-105.5));
#9132=CARTESIAN_POINT('Ctrl Pts',(43.6995308303615,15.6875,-105.5));
#9133=CARTESIAN_POINT('Ctrl Pts',(74.5997654151808,15.625,-74.5997654151808));
#9134=CARTESIAN_POINT('Ctrl Pts',(105.5,15.5625,-43.6995308303616));
#9135=CARTESIAN_POINT('Ctrl Pts',(105.5,15.5,-1.29200237310046E-14));
#9136=CARTESIAN_POINT('Ctrl Pts',(105.5,15.4375,43.6995308303615));
#9137=CARTESIAN_POINT('Ctrl Pts',(74.5997654151808,15.375,74.5997654151808));
#9138=CARTESIAN_POINT('Ctrl Pts',(43.6995308303616,15.3125,105.5));
#9139=CARTESIAN_POINT('Ctrl Pts',(1.93800355965069E-14,15.25,105.5));
#9140=CARTESIAN_POINT('Ctrl Pts',(-43.6995308303616,15.1875,105.5));
#9141=CARTESIAN_POINT('Ctrl Pts',(-74.5997654151808,15.125,74.5997654151808));
#9142=CARTESIAN_POINT('Ctrl Pts',(-105.5,15.0625,43.6995308303616));
#9143=CARTESIAN_POINT('Ctrl Pts',(-105.5,15.,0.));
#9144=CARTESIAN_POINT('Ctrl Pts',(-105.5,14.9375,-43.6995308303615));
#9145=CARTESIAN_POINT('Ctrl Pts',(-74.5997654151808,14.875,-74.5997654151808));
#9146=CARTESIAN_POINT('Ctrl Pts',(-43.6995308303615,14.8125,-105.5));
#9147=CARTESIAN_POINT('Ctrl Pts',(-6.46001186550229E-15,14.75,-105.5));
#9148=CARTESIAN_POINT('Ctrl Pts',(43.6995308303615,14.6875,-105.5));
#9149=CARTESIAN_POINT('Ctrl Pts',(74.5997654151808,14.625,-74.5997654151808));
#9150=CARTESIAN_POINT('Ctrl Pts',(105.5,14.5625,-43.6995308303616));
#9151=CARTESIAN_POINT('Ctrl Pts',(105.5,14.5,-1.29200237310046E-14));
#9152=CARTESIAN_POINT('Ctrl Pts',(105.5,14.4375,43.6995308303615));
#9153=CARTESIAN_POINT('Ctrl Pts',(74.5997654151808,14.375,74.5997654151808));
#9154=CARTESIAN_POINT('Ctrl Pts',(43.6995308303616,14.3125,105.5));
#9155=CARTESIAN_POINT('Ctrl Pts',(1.93800355965069E-14,14.25,105.5));
#9156=CARTESIAN_POINT('Ctrl Pts',(-43.6995308303616,14.1875,105.5));
#9157=CARTESIAN_POINT('Ctrl Pts',(-74.5997654151808,14.125,74.5997654151808));
#9158=CARTESIAN_POINT('Ctrl Pts',(-105.5,14.0625,43.6995308303616));
#9159=CARTESIAN_POINT('Ctrl Pts',(-105.5,14.,0.));
#9160=CARTESIAN_POINT('Ctrl Pts',(-105.5,13.9375,-43.6995308303615));
#9161=CARTESIAN_POINT('Ctrl Pts',(-74.5997654151808,13.875,-74.5997654151808));
#9162=CARTESIAN_POINT('Ctrl Pts',(-43.6995308303615,13.8125,-105.5));
#9163=CARTESIAN_POINT('Ctrl Pts',(-6.46001186550229E-15,13.75,-105.5));
#9164=CARTESIAN_POINT('Ctrl Pts',(43.6995308303615,13.6875,-105.5));
#9165=CARTESIAN_POINT('Ctrl Pts',(74.5997654151808,13.625,-74.5997654151808));
#9166=CARTESIAN_POINT('Ctrl Pts',(105.5,13.5625,-43.6995308303616));
#9167=CARTESIAN_POINT('Ctrl Pts',(105.5,13.5,-1.29200237310046E-14));
#9168=CARTESIAN_POINT('Ctrl Pts',(105.5,13.4375,43.6995308303615));
#9169=CARTESIAN_POINT('Ctrl Pts',(74.5997654151808,13.375,74.5997654151808));
#9170=CARTESIAN_POINT('Ctrl Pts',(43.6995308303616,13.3125,105.5));
#9171=CARTESIAN_POINT('Ctrl Pts',(1.93800355965069E-14,13.25,105.5));
#9172=CARTESIAN_POINT('Ctrl Pts',(-43.6995308303616,13.1875,105.5));
#9173=CARTESIAN_POINT('Ctrl Pts',(-74.5997654151808,13.125,74.5997654151808));
#9174=CARTESIAN_POINT('Ctrl Pts',(-105.5,13.0625,43.6995308303616));
#9175=CARTESIAN_POINT('Ctrl Pts',(-105.5,13.,0.));
#9176=CARTESIAN_POINT('Ctrl Pts',(-105.5,12.9375,-43.6995308303615));
#9177=CARTESIAN_POINT('Ctrl Pts',(-74.5997654151808,12.875,-74.5997654151808));
#9178=CARTESIAN_POINT('Ctrl Pts',(-43.6995308303615,12.8125,-105.5));
#9179=CARTESIAN_POINT('Ctrl Pts',(-6.46001186550229E-15,12.75,-105.5));
#9180=CARTESIAN_POINT('Ctrl Pts',(43.6995308303615,12.6875,-105.5));
#9181=CARTESIAN_POINT('Ctrl Pts',(74.5997654151808,12.625,-74.5997654151808));
#9182=CARTESIAN_POINT('Ctrl Pts',(105.5,12.5625,-43.6995308303616));
#9183=CARTESIAN_POINT('Ctrl Pts',(105.5,12.5,-1.29200237310046E-14));
#9184=CARTESIAN_POINT('Ctrl Pts',(105.5,12.4375,43.6995308303615));
#9185=CARTESIAN_POINT('Ctrl Pts',(74.5997654151808,12.375,74.5997654151808));
#9186=CARTESIAN_POINT('Ctrl Pts',(43.6995308303616,12.3125,105.5));
#9187=CARTESIAN_POINT('Ctrl Pts',(1.93800355965069E-14,12.25,105.5));
#9188=CARTESIAN_POINT('Ctrl Pts',(-43.6995308303616,12.1875,105.5));
#9189=CARTESIAN_POINT('Ctrl Pts',(-74.5997654151808,12.125,74.5997654151808));
#9190=CARTESIAN_POINT('Ctrl Pts',(-105.5,12.0625,43.6995308303616));
#9191=CARTESIAN_POINT('Ctrl Pts',(-105.5,12.,0.));
#9192=CARTESIAN_POINT('Ctrl Pts',(-105.5,11.9375,-43.6995308303615));
#9193=CARTESIAN_POINT('Ctrl Pts',(-74.5997654151808,11.875,-74.5997654151808));
#9194=CARTESIAN_POINT('Ctrl Pts',(-43.6995308303615,11.8125,-105.5));
#9195=CARTESIAN_POINT('Ctrl Pts',(-6.46001186550229E-15,11.75,-105.5));
#9196=CARTESIAN_POINT('Ctrl Pts',(43.6995308303615,11.6875,-105.5));
#9197=CARTESIAN_POINT('Ctrl Pts',(74.5997654151808,11.625,-74.5997654151808));
#9198=CARTESIAN_POINT('Ctrl Pts',(105.5,11.5625,-43.6995308303616));
#9199=CARTESIAN_POINT('Ctrl Pts',(105.5,11.5,-1.29200237310046E-14));
#9200=CARTESIAN_POINT('Ctrl Pts',(105.5,11.4375,43.6995308303615));
#9201=CARTESIAN_POINT('Ctrl Pts',(74.5997654151808,11.375,74.5997654151808));
#9202=CARTESIAN_POINT('Ctrl Pts',(43.6995308303616,11.3125,105.5));
#9203=CARTESIAN_POINT('Ctrl Pts',(1.93800355965069E-14,11.25,105.5));
#9204=CARTESIAN_POINT('Ctrl Pts',(-43.6995308303616,11.1875,105.5));
#9205=CARTESIAN_POINT('Ctrl Pts',(-74.5997654151808,11.125,74.5997654151808));
#9206=CARTESIAN_POINT('Ctrl Pts',(-105.5,11.0625,43.6995308303616));
#9207=CARTESIAN_POINT('Ctrl Pts',(-105.5,11.,0.));
#9208=CARTESIAN_POINT('Ctrl Pts',(-105.5,10.9375,-43.6995308303615));
#9209=CARTESIAN_POINT('Ctrl Pts',(-74.5997654151808,10.875,-74.5997654151808));
#9210=CARTESIAN_POINT('Ctrl Pts',(-43.6995308303615,10.8125,-105.5));
#9211=CARTESIAN_POINT('Ctrl Pts',(-6.46001186550229E-15,10.75,-105.5));
#9212=CARTESIAN_POINT('Ctrl Pts',(43.6995308303615,10.6875,-105.5));
#9213=CARTESIAN_POINT('Ctrl Pts',(74.5997654151808,10.625,-74.5997654151808));
#9214=CARTESIAN_POINT('Ctrl Pts',(105.5,10.5625,-43.6995308303616));
#9215=CARTESIAN_POINT('Ctrl Pts',(105.5,10.5,-1.29200237310046E-14));
#9216=CARTESIAN_POINT('Ctrl Pts',(105.5,10.4375,43.6995308303615));
#9217=CARTESIAN_POINT('Ctrl Pts',(74.5997654151808,10.375,74.5997654151808));
#9218=CARTESIAN_POINT('Ctrl Pts',(43.6995308303616,10.3125,105.5));
#9219=CARTESIAN_POINT('Ctrl Pts',(1.93800355965069E-14,10.25,105.5));
#9220=CARTESIAN_POINT('Ctrl Pts',(-43.6995308303616,10.1875,105.5));
#9221=CARTESIAN_POINT('Ctrl Pts',(-74.5997654151808,10.125,74.5997654151808));
#9222=CARTESIAN_POINT('Ctrl Pts',(-105.5,10.0625,43.6995308303616));
#9223=CARTESIAN_POINT('Ctrl Pts',(-105.5,9.99999999999999,0.));
#9224=CARTESIAN_POINT('Ctrl Pts',(-105.5,9.93749999999999,-43.6995308303615));
#9225=CARTESIAN_POINT('Ctrl Pts',(-74.5997654151808,9.87499999999999,-74.5997654151808));
#9226=CARTESIAN_POINT('Ctrl Pts',(-43.6995308303615,9.81249999999999,-105.5));
#9227=CARTESIAN_POINT('Ctrl Pts',(-6.46001186550229E-15,9.74999999999999,
-105.5));
#9228=CARTESIAN_POINT('Ctrl Pts',(43.6995308303615,9.68749999999999,-105.5));
#9229=CARTESIAN_POINT('Ctrl Pts',(74.5997654151808,9.62499999999999,-74.5997654151808));
#9230=CARTESIAN_POINT('Ctrl Pts',(105.5,9.56249999999999,-43.6995308303616));
#9231=CARTESIAN_POINT('Ctrl Pts',(105.5,9.49999999999999,-1.29200237310046E-14));
#9232=CARTESIAN_POINT('Ctrl Pts',(105.5,9.43749999999999,43.6995308303615));
#9233=CARTESIAN_POINT('Ctrl Pts',(74.5997654151808,9.37499999999999,74.5997654151808));
#9234=CARTESIAN_POINT('Ctrl Pts',(43.6995308303616,9.31249999999999,105.5));
#9235=CARTESIAN_POINT('Ctrl Pts',(1.93800355965069E-14,9.24999999999999,
105.5));
#9236=CARTESIAN_POINT('Ctrl Pts',(-43.6995308303616,9.18749999999999,105.5));
#9237=CARTESIAN_POINT('Ctrl Pts',(-74.5997654151808,9.12499999999999,74.5997654151808));
#9238=CARTESIAN_POINT('Ctrl Pts',(-105.5,9.06249999999999,43.6995308303616));
#9239=CARTESIAN_POINT('Ctrl Pts',(-105.5,8.99999999999999,0.));
#9240=CARTESIAN_POINT('Ctrl Pts',(-105.5,8.93749999999999,-43.6995308303615));
#9241=CARTESIAN_POINT('Ctrl Pts',(-74.5997654151808,8.87499999999999,-74.5997654151808));
#9242=CARTESIAN_POINT('Ctrl Pts',(-43.6995308303615,8.81249999999999,-105.5));
#9243=CARTESIAN_POINT('Ctrl Pts',(-6.46001186550229E-15,8.74999999999999,
-105.5));
#9244=CARTESIAN_POINT('Ctrl Pts',(43.6995308303615,8.68749999999999,-105.5));
#9245=CARTESIAN_POINT('Ctrl Pts',(74.5997654151808,8.62499999999999,-74.5997654151808));
#9246=CARTESIAN_POINT('Ctrl Pts',(105.5,8.56249999999999,-43.6995308303616));
#9247=CARTESIAN_POINT('Ctrl Pts',(105.5,8.49999999999999,-1.29200237310046E-14));
#9248=CARTESIAN_POINT('Ctrl Pts',(105.5,8.43749999999999,43.6995308303615));
#9249=CARTESIAN_POINT('Ctrl Pts',(74.5997654151808,8.37499999999999,74.5997654151808));
#9250=CARTESIAN_POINT('Ctrl Pts',(43.6995308303616,8.31249999999999,105.5));
#9251=CARTESIAN_POINT('Ctrl Pts',(1.93800355965069E-14,8.24999999999999,
105.5));
#9252=CARTESIAN_POINT('Ctrl Pts',(-43.6995308303616,8.18749999999999,105.5));
#9253=CARTESIAN_POINT('Ctrl Pts',(-74.5997654151808,8.12499999999999,74.5997654151808));
#9254=CARTESIAN_POINT('Ctrl Pts',(-105.5,8.06249999999999,43.6995308303616));
#9255=CARTESIAN_POINT('Ctrl Pts',(-105.5,7.99999999999999,0.));
#9256=CARTESIAN_POINT('Ctrl Pts',(-105.5,7.93749999999999,-43.6995308303615));
#9257=CARTESIAN_POINT('Ctrl Pts',(-74.5997654151808,7.87499999999999,-74.5997654151808));
#9258=CARTESIAN_POINT('Ctrl Pts',(-43.6995308303615,7.81249999999999,-105.5));
#9259=CARTESIAN_POINT('Ctrl Pts',(-6.46001186550229E-15,7.74999999999999,
-105.5));
#9260=CARTESIAN_POINT('Ctrl Pts',(43.6995308303615,7.68749999999999,-105.5));
#9261=CARTESIAN_POINT('Ctrl Pts',(74.5997654151808,7.62499999999999,-74.5997654151808));
#9262=CARTESIAN_POINT('Ctrl Pts',(105.5,7.56249999999999,-43.6995308303616));
#9263=CARTESIAN_POINT('Ctrl Pts',(105.5,7.49999999999999,-1.29200237310046E-14));
#9264=CARTESIAN_POINT('Ctrl Pts',(105.5,7.43749999999999,43.6995308303615));
#9265=CARTESIAN_POINT('Ctrl Pts',(74.5997654151808,7.37499999999999,74.5997654151808));
#9266=CARTESIAN_POINT('Ctrl Pts',(43.6995308303616,7.31249999999999,105.5));
#9267=CARTESIAN_POINT('Ctrl Pts',(1.93800355965069E-14,7.24999999999999,
105.5));
#9268=CARTESIAN_POINT('Ctrl Pts',(-43.6995308303616,7.18749999999999,105.5));
#9269=CARTESIAN_POINT('Ctrl Pts',(-74.5997654151808,7.12499999999999,74.5997654151808));
#9270=CARTESIAN_POINT('Ctrl Pts',(-105.5,7.06249999999998,43.6995308303616));
#9271=CARTESIAN_POINT('Ctrl Pts',(-105.5,6.99999999999998,0.));
#9272=CARTESIAN_POINT('Ctrl Pts',(-105.5,6.93749999999999,-43.6995308303615));
#9273=CARTESIAN_POINT('Ctrl Pts',(-74.5997654151808,6.87499999999999,-74.5997654151808));
#9274=CARTESIAN_POINT('Ctrl Pts',(-43.6995308303615,6.81249999999999,-105.5));
#9275=CARTESIAN_POINT('Ctrl Pts',(-6.46001186550229E-15,6.74999999999998,
-105.5));
#9276=CARTESIAN_POINT('Ctrl Pts',(43.6995308303615,6.68749999999998,-105.5));
#9277=CARTESIAN_POINT('Ctrl Pts',(74.5997654151808,6.62499999999999,-74.5997654151808));
#9278=CARTESIAN_POINT('Ctrl Pts',(105.5,6.56249999999998,-43.6995308303616));
#9279=CARTESIAN_POINT('Ctrl Pts',(105.5,6.49999999999998,-1.29200237310046E-14));
#9280=CARTESIAN_POINT('Ctrl Pts',(105.5,6.43749999999998,43.6995308303615));
#9281=CARTESIAN_POINT('Ctrl Pts',(74.5997654151808,6.37499999999998,74.5997654151808));
#9282=CARTESIAN_POINT('Ctrl Pts',(43.6995308303616,6.31249999999999,105.5));
#9283=CARTESIAN_POINT('Ctrl Pts',(1.93800355965069E-14,6.24999999999998,
105.5));
#9284=CARTESIAN_POINT('Ctrl Pts',(-43.6995308303616,6.18749999999998,105.5));
#9285=CARTESIAN_POINT('Ctrl Pts',(-74.5997654151808,6.12499999999998,74.5997654151808));
#9286=CARTESIAN_POINT('Ctrl Pts',(-105.5,6.06249999999998,43.6995308303616));
#9287=CARTESIAN_POINT('Ctrl Pts',(-105.5,5.99999999999999,0.));
#9288=CARTESIAN_POINT('Ctrl Pts',(-105.5,5.93749999999999,-43.6995308303615));
#9289=CARTESIAN_POINT('Ctrl Pts',(-74.5997654151808,5.87499999999999,-74.5997654151808));
#9290=CARTESIAN_POINT('Ctrl Pts',(-43.6995308303615,5.81249999999999,-105.5));
#9291=CARTESIAN_POINT('Ctrl Pts',(-6.46001186550229E-15,5.74999999999999,
-105.5));
#9292=CARTESIAN_POINT('Ctrl Pts',(43.6995308303615,5.68749999999999,-105.5));
#9293=CARTESIAN_POINT('Ctrl Pts',(74.5997654151808,5.62499999999999,-74.5997654151808));
#9294=CARTESIAN_POINT('Ctrl Pts',(105.5,5.56249999999999,-43.6995308303616));
#9295=CARTESIAN_POINT('Ctrl Pts',(105.5,5.49999999999999,-1.29200237310046E-14));
#9296=CARTESIAN_POINT('Ctrl Pts',(105.5,5.43749999999999,43.6995308303615));
#9297=CARTESIAN_POINT('Ctrl Pts',(74.5997654151808,5.37499999999999,74.5997654151808));
#9298=CARTESIAN_POINT('Ctrl Pts',(43.6995308303616,5.31249999999999,105.5));
#9299=CARTESIAN_POINT('Ctrl Pts',(1.93800355965069E-14,5.24999999999999,
105.5));
#9300=CARTESIAN_POINT('Ctrl Pts',(-43.6995308303616,5.18749999999999,105.5));
#9301=CARTESIAN_POINT('Ctrl Pts',(-74.5997654151808,5.12499999999999,74.5997654151808));
#9302=CARTESIAN_POINT('Ctrl Pts',(-105.5,5.06249999999999,43.6995308303616));
#9303=CARTESIAN_POINT('Ctrl Pts',(-105.5,4.99999999999999,0.));
#9304=CARTESIAN_POINT('Ctrl Pts',(-105.5,4.93749999999999,-43.6995308303615));
#9305=CARTESIAN_POINT('Ctrl Pts',(-74.5997654151808,4.87499999999999,-74.5997654151808));
#9306=CARTESIAN_POINT('Ctrl Pts',(-43.6995308303615,4.81249999999999,-105.5));
#9307=CARTESIAN_POINT('Ctrl Pts',(-6.46001186550229E-15,4.74999999999999,
-105.5));
#9308=CARTESIAN_POINT('Ctrl Pts',(43.6995308303615,4.68749999999999,-105.5));
#9309=CARTESIAN_POINT('Ctrl Pts',(74.5997654151808,4.62499999999999,-74.5997654151808));
#9310=CARTESIAN_POINT('Ctrl Pts',(105.5,4.56249999999999,-43.6995308303616));
#9311=CARTESIAN_POINT('Ctrl Pts',(105.5,4.49999999999999,-1.29200237310046E-14));
#9312=CARTESIAN_POINT('Ctrl Pts',(105.5,4.43749999999999,43.6995308303615));
#9313=CARTESIAN_POINT('Ctrl Pts',(74.5997654151808,4.37499999999999,74.5997654151808));
#9314=CARTESIAN_POINT('Ctrl Pts',(43.6995308303616,4.31249999999999,105.5));
#9315=CARTESIAN_POINT('Ctrl Pts',(1.93800355965069E-14,4.24999999999999,
105.5));
#9316=CARTESIAN_POINT('Ctrl Pts',(-43.6995308303616,4.18749999999999,105.5));
#9317=CARTESIAN_POINT('Ctrl Pts',(-74.5997654151808,4.12499999999999,74.5997654151808));
#9318=CARTESIAN_POINT('Ctrl Pts',(-105.5,4.06249999999999,43.6995308303616));
#9319=CARTESIAN_POINT('Ctrl Pts',(-105.5,3.99999999999999,0.));
#9320=CARTESIAN_POINT('Ctrl Pts',(-105.5,3.93749999999999,-43.6995308303615));
#9321=CARTESIAN_POINT('Ctrl Pts',(-74.5997654151808,3.87499999999999,-74.5997654151808));
#9322=CARTESIAN_POINT('Ctrl Pts',(-43.6995308303615,3.81249999999999,-105.5));
#9323=CARTESIAN_POINT('Ctrl Pts',(-6.46001186550229E-15,3.74999999999999,
-105.5));
#9324=CARTESIAN_POINT('Ctrl Pts',(43.6995308303615,3.68749999999999,-105.5));
#9325=CARTESIAN_POINT('Ctrl Pts',(74.5997654151808,3.62499999999999,-74.5997654151808));
#9326=CARTESIAN_POINT('Ctrl Pts',(105.5,3.56249999999999,-43.6995308303616));
#9327=CARTESIAN_POINT('Ctrl Pts',(105.5,3.49999999999999,-1.29200237310046E-14));
#9328=CARTESIAN_POINT('Ctrl Pts',(105.5,3.43749999999999,43.6995308303615));
#9329=CARTESIAN_POINT('Ctrl Pts',(74.5997654151808,3.37499999999999,74.5997654151808));
#9330=CARTESIAN_POINT('Ctrl Pts',(43.6995308303616,3.31249999999999,105.5));
#9331=CARTESIAN_POINT('Ctrl Pts',(1.93800355965069E-14,3.24999999999999,
105.5));
#9332=CARTESIAN_POINT('Ctrl Pts',(-43.6995308303616,3.18749999999999,105.5));
#9333=CARTESIAN_POINT('Ctrl Pts',(-74.5997654151808,3.12499999999999,74.5997654151808));
#9334=CARTESIAN_POINT('Ctrl Pts',(-105.5,3.06249999999999,43.6995308303616));
#9335=CARTESIAN_POINT('Ctrl Pts',(-105.5,2.99999999999999,0.));
#9336=CARTESIAN_POINT('Ctrl Pts',(-105.5,2.93749999999999,-43.6995308303615));
#9337=CARTESIAN_POINT('Ctrl Pts',(-74.5997654151808,2.87499999999999,-74.5997654151808));
#9338=CARTESIAN_POINT('Ctrl Pts',(-43.6995308303615,2.81249999999999,-105.5));
#9339=CARTESIAN_POINT('Ctrl Pts',(-6.46001186550229E-15,2.74999999999999,
-105.5));
#9340=CARTESIAN_POINT('Ctrl Pts',(43.6995308303615,2.68749999999999,-105.5));
#9341=CARTESIAN_POINT('Ctrl Pts',(74.5997654151808,2.62499999999999,-74.5997654151808));
#9342=CARTESIAN_POINT('Ctrl Pts',(105.5,2.56249999999999,-43.6995308303616));
#9343=CARTESIAN_POINT('Ctrl Pts',(105.5,2.49999999999999,-1.29200237310046E-14));
#9344=CARTESIAN_POINT('Ctrl Pts',(105.5,2.43749999999999,43.6995308303615));
#9345=CARTESIAN_POINT('Ctrl Pts',(74.5997654151808,2.37499999999999,74.5997654151808));
#9346=CARTESIAN_POINT('Ctrl Pts',(43.6995308303616,2.31249999999999,105.5));
#9347=CARTESIAN_POINT('Ctrl Pts',(1.93800355965069E-14,2.24999999999999,
105.5));
#9348=CARTESIAN_POINT('Ctrl Pts',(-43.6995308303616,2.18749999999999,105.5));
#9349=CARTESIAN_POINT('Ctrl Pts',(-74.5997654151808,2.12499999999999,74.5997654151808));
#9350=CARTESIAN_POINT('Ctrl Pts',(-105.5,2.06249999999999,43.6995308303616));
#9351=CARTESIAN_POINT('Ctrl Pts',(-105.5,1.99999999999999,0.));
#9352=CARTESIAN_POINT('Ctrl Pts',(-105.5,1.93749999999999,-43.6995308303615));
#9353=CARTESIAN_POINT('Ctrl Pts',(-74.5997654151808,1.87499999999999,-74.5997654151808));
#9354=CARTESIAN_POINT('Ctrl Pts',(-43.6995308303615,1.81249999999999,-105.5));
#9355=CARTESIAN_POINT('Ctrl Pts',(-6.46001186550229E-15,1.74999999999999,
-105.5));
#9356=CARTESIAN_POINT('Ctrl Pts',(43.6995308303615,1.68749999999999,-105.5));
#9357=CARTESIAN_POINT('Ctrl Pts',(74.5997654151808,1.62499999999999,-74.5997654151808));
#9358=CARTESIAN_POINT('Ctrl Pts',(105.5,1.56249999999999,-43.6995308303616));
#9359=CARTESIAN_POINT('Ctrl Pts',(105.5,1.49999999999999,-1.29200237310046E-14));
#9360=CARTESIAN_POINT('Ctrl Pts',(105.5,1.43749999999999,43.6995308303615));
#9361=CARTESIAN_POINT('Ctrl Pts',(74.5997654151808,1.37499999999999,74.5997654151808));
#9362=CARTESIAN_POINT('Ctrl Pts',(43.6995308303616,1.31249999999999,105.5));
#9363=CARTESIAN_POINT('Ctrl Pts',(1.93800355965069E-14,1.24999999999999,
105.5));
#9364=CARTESIAN_POINT('Ctrl Pts',(-43.6995308303616,1.18749999999999,105.5));
#9365=CARTESIAN_POINT('Ctrl Pts',(-74.5997654151808,1.12499999999999,74.5997654151808));
#9366=CARTESIAN_POINT('Ctrl Pts',(-105.5,1.06249999999999,43.6995308303616));
#9367=CARTESIAN_POINT('Ctrl Pts',(-105.5,0.999999999999987,0.));
#9368=CARTESIAN_POINT('Ctrl Pts',(-105.5,0.937499999999987,-43.6995308303615));
#9369=CARTESIAN_POINT('Ctrl Pts',(-74.5997654151808,0.874999999999987,-74.5997654151808));
#9370=CARTESIAN_POINT('Ctrl Pts',(-43.6995308303615,0.812499999999987,-105.5));
#9371=CARTESIAN_POINT('Ctrl Pts',(-6.46001186550229E-15,0.749999999999987,
-105.5));
#9372=CARTESIAN_POINT('Ctrl Pts',(43.6995308303615,0.687499999999987,-105.5));
#9373=CARTESIAN_POINT('Ctrl Pts',(74.5997654151808,0.624999999999987,-74.5997654151808));
#9374=CARTESIAN_POINT('Ctrl Pts',(105.5,0.562499999999987,-43.6995308303616));
#9375=CARTESIAN_POINT('Ctrl Pts',(105.5,0.499999999999987,-1.29200237310046E-14));
#9376=CARTESIAN_POINT('Ctrl Pts',(105.5,0.437499999999987,43.6995308303615));
#9377=CARTESIAN_POINT('Ctrl Pts',(74.5997654151808,0.374999999999986,74.5997654151808));
#9378=CARTESIAN_POINT('Ctrl Pts',(43.6995308303616,0.312499999999986,105.5));
#9379=CARTESIAN_POINT('Ctrl Pts',(1.93800355965069E-14,0.249999999999986,
105.5));
#9380=CARTESIAN_POINT('Ctrl Pts',(-43.6995308303616,0.187499999999986,105.5));
#9381=CARTESIAN_POINT('Ctrl Pts',(-74.5997654151808,0.124999999999986,74.5997654151808));
#9382=CARTESIAN_POINT('Ctrl Pts',(-105.5,0.0624999999999862,43.6995308303616));
#9383=CARTESIAN_POINT('Ctrl Pts',(-105.5,-1.38777878078145E-14,0.));
#9384=CARTESIAN_POINT('Ctrl Pts',(104.958734125,49.1875000013656,-1.28537377788739E-14));
#9385=CARTESIAN_POINT('Ctrl Pts',(104.958734125,49.1250000013656,43.4753311640868));
#9386=CARTESIAN_POINT('Ctrl Pts',(74.2170326445434,49.0625000013656,74.2170326445434));
#9387=CARTESIAN_POINT('Ctrl Pts',(43.4753311640869,49.0000000013656,104.958734125));
#9388=CARTESIAN_POINT('Ctrl Pts',(1.92806066683109E-14,48.9375000013656,
104.958734125));
#9389=CARTESIAN_POINT('Ctrl Pts',(-43.4753311640868,48.8750000013656,104.958734125));
#9390=CARTESIAN_POINT('Ctrl Pts',(-74.2170326445434,48.8125000013656,74.2170326445434));
#9391=CARTESIAN_POINT('Ctrl Pts',(-104.958734125,48.7500000013656,43.4753311640869));
#9392=CARTESIAN_POINT('Ctrl Pts',(-104.958734125,48.6875000013656,0.));
#9393=CARTESIAN_POINT('Ctrl Pts',(-104.958734125,48.6250000013656,-43.4753311640868));
#9394=CARTESIAN_POINT('Ctrl Pts',(-74.2170326445434,48.5625000013656,-74.2170326445434));
#9395=CARTESIAN_POINT('Ctrl Pts',(-43.4753311640868,48.5000000013656,-104.958734125));
#9396=CARTESIAN_POINT('Ctrl Pts',(-6.42686888943697E-15,48.4375000013656,
-104.958734125));
#9397=CARTESIAN_POINT('Ctrl Pts',(43.4753311640868,48.3750000013656,-104.958734125));
#9398=CARTESIAN_POINT('Ctrl Pts',(74.2170326445434,48.3125000013656,-74.2170326445434));
#9399=CARTESIAN_POINT('Ctrl Pts',(104.958734125,48.2500000013656,-43.4753311640868));
#9400=CARTESIAN_POINT('Ctrl Pts',(104.958734125,48.1875000013656,-1.28537377788739E-14));
#9401=CARTESIAN_POINT('Origin',(-7.105427357601E-14,49.5625000013656,-6.0924204042587E-14));
#9402=CARTESIAN_POINT('Ctrl Pts',(104.958734125,48.9375000013656,-1.28537377788739E-14));
#9403=CARTESIAN_POINT('Ctrl Pts',(104.958734125,48.8750000013656,43.4753311640868));
#9404=CARTESIAN_POINT('Ctrl Pts',(74.2170326445434,48.8125000013656,74.2170326445434));
#9405=CARTESIAN_POINT('Ctrl Pts',(43.4753311640869,48.7500000013656,104.958734125));
#9406=CARTESIAN_POINT('Ctrl Pts',(1.92806066683109E-14,48.6875000013656,
104.958734125));
#9407=CARTESIAN_POINT('Ctrl Pts',(-43.4753311640868,48.6250000013656,104.958734125));
#9408=CARTESIAN_POINT('Ctrl Pts',(-74.2170326445434,48.5625000013656,74.2170326445434));
#9409=CARTESIAN_POINT('Ctrl Pts',(-104.958734125,48.5000000013656,43.4753311640869));
#9410=CARTESIAN_POINT('Ctrl Pts',(-104.958734125,48.4375000013656,0.));
#9411=CARTESIAN_POINT('Ctrl Pts',(-104.958734125,48.3750000013656,-43.4753311640868));
#9412=CARTESIAN_POINT('Ctrl Pts',(-74.2170326445434,48.3125000013656,-74.2170326445434));
#9413=CARTESIAN_POINT('Ctrl Pts',(-43.4753311640868,48.2500000013656,-104.958734125));
#9414=CARTESIAN_POINT('Ctrl Pts',(-6.42686888943697E-15,48.1875000013656,
-104.958734125));
#9415=CARTESIAN_POINT('Ctrl Pts',(43.4753311640868,48.1250000013656,-104.958734125));
#9416=CARTESIAN_POINT('Ctrl Pts',(74.2170326445434,48.0625000013656,-74.2170326445434));
#9417=CARTESIAN_POINT('Ctrl Pts',(104.958734125,48.0000000013656,-43.4753311640868));
#9418=CARTESIAN_POINT('Ctrl Pts',(104.958734125,47.9375000013656,-1.28537377788739E-14));
#9419=CARTESIAN_POINT('Ctrl Pts',(-105.5,49.1250000027312,0.));
#9420=CARTESIAN_POINT('Ctrl Pts',(-105.5,49.0625000027312,-43.6995308303615));
#9421=CARTESIAN_POINT('Ctrl Pts',(-74.5997654151808,49.0000000027312,-74.5997654151808));
#9422=CARTESIAN_POINT('Ctrl Pts',(-43.6995308303615,48.9375000027312,-105.5));
#9423=CARTESIAN_POINT('Ctrl Pts',(-6.46001186550229E-15,48.8750000027312,
-105.5));
#9424=CARTESIAN_POINT('Ctrl Pts',(43.6995308303615,48.8125000027312,-105.5));
#9425=CARTESIAN_POINT('Ctrl Pts',(74.5997654151808,48.7500000027312,-74.5997654151808));
#9426=CARTESIAN_POINT('Ctrl Pts',(105.5,48.6875000027312,-43.6995308303616));
#9427=CARTESIAN_POINT('Ctrl Pts',(105.5,48.6250000027312,-1.29200237310046E-14));
#9428=CARTESIAN_POINT('Ctrl Pts',(105.5,48.5625000027312,43.6995308303615));
#9429=CARTESIAN_POINT('Ctrl Pts',(74.5997654151808,48.5000000027312,74.5997654151808));
#9430=CARTESIAN_POINT('Ctrl Pts',(43.6995308303616,48.4375000027312,105.5));
#9431=CARTESIAN_POINT('Ctrl Pts',(1.93800355965069E-14,48.3750000027312,
105.5));
#9432=CARTESIAN_POINT('Ctrl Pts',(-43.6995308303616,48.3125000027312,105.5));
#9433=CARTESIAN_POINT('Ctrl Pts',(-74.5997654151808,48.2500000027312,74.5997654151808));
#9434=CARTESIAN_POINT('Ctrl Pts',(-105.5,48.1875000027312,43.6995308303616));
#9435=CARTESIAN_POINT('Ctrl Pts',(-105.5,48.1250000027312,0.));
#9436=CARTESIAN_POINT('Ctrl Pts',(-105.5,48.0625000027312,-43.6995308303615));
#9437=CARTESIAN_POINT('Ctrl Pts',(-74.5997654151808,48.0000000027312,-74.5997654151808));
#9438=CARTESIAN_POINT('Ctrl Pts',(-43.6995308303615,47.9375000027312,-105.5));
#9439=CARTESIAN_POINT('Ctrl Pts',(-6.46001186550229E-15,47.8750000027312,
-105.5));
#9440=CARTESIAN_POINT('Ctrl Pts',(43.6995308303615,47.8125000027312,-105.5));
#9441=CARTESIAN_POINT('Ctrl Pts',(74.5997654151808,47.7500000027312,-74.5997654151808));
#9442=CARTESIAN_POINT('Ctrl Pts',(105.5,47.6875000027312,-43.6995308303616));
#9443=CARTESIAN_POINT('Ctrl Pts',(105.5,47.6250000027312,-1.29200237310046E-14));
#9444=CARTESIAN_POINT('Ctrl Pts',(105.5,47.5625000027312,43.6995308303615));
#9445=CARTESIAN_POINT('Ctrl Pts',(74.5997654151808,47.5000000027312,74.5997654151808));
#9446=CARTESIAN_POINT('Ctrl Pts',(43.6995308303616,47.4375000027312,105.5));
#9447=CARTESIAN_POINT('Ctrl Pts',(1.93800355965069E-14,47.3750000027312,
105.5));
#9448=CARTESIAN_POINT('Ctrl Pts',(-43.6995308303616,47.3125000027312,105.5));
#9449=CARTESIAN_POINT('Ctrl Pts',(-74.5997654151808,47.2500000027312,74.5997654151808));
#9450=CARTESIAN_POINT('Ctrl Pts',(-105.5,47.1875000027312,43.6995308303616));
#9451=CARTESIAN_POINT('Ctrl Pts',(-105.5,47.1250000027312,0.));
#9452=CARTESIAN_POINT('Ctrl Pts',(-105.5,47.0625000027312,-43.6995308303615));
#9453=CARTESIAN_POINT('Ctrl Pts',(-74.5997654151808,47.0000000027312,-74.5997654151808));
#9454=CARTESIAN_POINT('Ctrl Pts',(-43.6995308303615,46.9375000027312,-105.5));
#9455=CARTESIAN_POINT('Ctrl Pts',(-6.46001186550229E-15,46.8750000027312,
-105.5));
#9456=CARTESIAN_POINT('Ctrl Pts',(43.6995308303615,46.8125000027312,-105.5));
#9457=CARTESIAN_POINT('Ctrl Pts',(74.5997654151808,46.7500000027312,-74.5997654151808));
#9458=CARTESIAN_POINT('Ctrl Pts',(105.5,46.6875000027312,-43.6995308303616));
#9459=CARTESIAN_POINT('Ctrl Pts',(105.5,46.6250000027312,-1.29200237310046E-14));
#9460=CARTESIAN_POINT('Ctrl Pts',(105.5,46.5625000027312,43.6995308303615));
#9461=CARTESIAN_POINT('Ctrl Pts',(74.5997654151808,46.5000000027312,74.5997654151808));
#9462=CARTESIAN_POINT('Ctrl Pts',(43.6995308303616,46.4375000027312,105.5));
#9463=CARTESIAN_POINT('Ctrl Pts',(1.93800355965069E-14,46.3750000027312,
105.5));
#9464=CARTESIAN_POINT('Ctrl Pts',(-43.6995308303616,46.3125000027312,105.5));
#9465=CARTESIAN_POINT('Ctrl Pts',(-74.5997654151808,46.2500000027312,74.5997654151808));
#9466=CARTESIAN_POINT('Ctrl Pts',(-105.5,46.1875000027312,43.6995308303616));
#9467=CARTESIAN_POINT('Ctrl Pts',(-105.5,46.1250000027312,0.));
#9468=CARTESIAN_POINT('Ctrl Pts',(-105.5,46.0625000027312,-43.6995308303615));
#9469=CARTESIAN_POINT('Ctrl Pts',(-74.5997654151808,46.0000000027312,-74.5997654151808));
#9470=CARTESIAN_POINT('Ctrl Pts',(-43.6995308303615,45.9375000027312,-105.5));
#9471=CARTESIAN_POINT('Ctrl Pts',(-6.46001186550229E-15,45.8750000027312,
-105.5));
#9472=CARTESIAN_POINT('Ctrl Pts',(43.6995308303615,45.8125000027312,-105.5));
#9473=CARTESIAN_POINT('Ctrl Pts',(74.5997654151808,45.7500000027312,-74.5997654151808));
#9474=CARTESIAN_POINT('Ctrl Pts',(105.5,45.6875000027312,-43.6995308303616));
#9475=CARTESIAN_POINT('Ctrl Pts',(105.5,45.6250000027312,-1.29200237310046E-14));
#9476=CARTESIAN_POINT('Ctrl Pts',(105.5,45.5625000027312,43.6995308303615));
#9477=CARTESIAN_POINT('Ctrl Pts',(74.5997654151808,45.5000000027312,74.5997654151808));
#9478=CARTESIAN_POINT('Ctrl Pts',(43.6995308303616,45.4375000027312,105.5));
#9479=CARTESIAN_POINT('Ctrl Pts',(1.93800355965069E-14,45.3750000027312,
105.5));
#9480=CARTESIAN_POINT('Ctrl Pts',(-43.6995308303616,45.3125000027312,105.5));
#9481=CARTESIAN_POINT('Ctrl Pts',(-74.5997654151808,45.2500000027312,74.5997654151808));
#9482=CARTESIAN_POINT('Ctrl Pts',(-105.5,45.1875000027312,43.6995308303616));
#9483=CARTESIAN_POINT('Ctrl Pts',(-105.5,45.1250000027312,0.));
#9484=CARTESIAN_POINT('Ctrl Pts',(-105.5,45.0625000027312,-43.6995308303615));
#9485=CARTESIAN_POINT('Ctrl Pts',(-74.5997654151808,45.0000000027312,-74.5997654151808));
#9486=CARTESIAN_POINT('Ctrl Pts',(-43.6995308303615,44.9375000027312,-105.5));
#9487=CARTESIAN_POINT('Ctrl Pts',(-6.46001186550229E-15,44.8750000027312,
-105.5));
#9488=CARTESIAN_POINT('Ctrl Pts',(43.6995308303615,44.8125000027312,-105.5));
#9489=CARTESIAN_POINT('Ctrl Pts',(74.5997654151808,44.7500000027312,-74.5997654151808));
#9490=CARTESIAN_POINT('Ctrl Pts',(105.5,44.6875000027312,-43.6995308303616));
#9491=CARTESIAN_POINT('Ctrl Pts',(105.5,44.6250000027312,-1.29200237310046E-14));
#9492=CARTESIAN_POINT('Ctrl Pts',(105.5,44.5625000027312,43.6995308303615));
#9493=CARTESIAN_POINT('Ctrl Pts',(74.5997654151808,44.5000000027312,74.5997654151808));
#9494=CARTESIAN_POINT('Ctrl Pts',(43.6995308303616,44.4375000027312,105.5));
#9495=CARTESIAN_POINT('Ctrl Pts',(1.93800355965069E-14,44.3750000027312,
105.5));
#9496=CARTESIAN_POINT('Ctrl Pts',(-43.6995308303616,44.3125000027312,105.5));
#9497=CARTESIAN_POINT('Ctrl Pts',(-74.5997654151808,44.2500000027312,74.5997654151808));
#9498=CARTESIAN_POINT('Ctrl Pts',(-105.5,44.1875000027312,43.6995308303616));
#9499=CARTESIAN_POINT('Ctrl Pts',(-105.5,44.1250000027312,0.));
#9500=CARTESIAN_POINT('Ctrl Pts',(-105.5,44.0625000027312,-43.6995308303615));
#9501=CARTESIAN_POINT('Ctrl Pts',(-74.5997654151808,44.0000000027312,-74.5997654151808));
#9502=CARTESIAN_POINT('Ctrl Pts',(-43.6995308303615,43.9375000027312,-105.5));
#9503=CARTESIAN_POINT('Ctrl Pts',(-6.46001186550229E-15,43.8750000027312,
-105.5));
#9504=CARTESIAN_POINT('Ctrl Pts',(43.6995308303615,43.8125000027312,-105.5));
#9505=CARTESIAN_POINT('Ctrl Pts',(74.5997654151808,43.7500000027312,-74.5997654151808));
#9506=CARTESIAN_POINT('Ctrl Pts',(105.5,43.6875000027312,-43.6995308303616));
#9507=CARTESIAN_POINT('Ctrl Pts',(105.5,43.6250000027312,-1.29200237310046E-14));
#9508=CARTESIAN_POINT('Ctrl Pts',(105.5,43.5625000027312,43.6995308303615));
#9509=CARTESIAN_POINT('Ctrl Pts',(74.5997654151808,43.5000000027312,74.5997654151808));
#9510=CARTESIAN_POINT('Ctrl Pts',(43.6995308303616,43.4375000027312,105.5));
#9511=CARTESIAN_POINT('Ctrl Pts',(1.93800355965069E-14,43.3750000027312,
105.5));
#9512=CARTESIAN_POINT('Ctrl Pts',(-43.6995308303616,43.3125000027312,105.5));
#9513=CARTESIAN_POINT('Ctrl Pts',(-74.5997654151808,43.2500000027312,74.5997654151808));
#9514=CARTESIAN_POINT('Ctrl Pts',(-105.5,43.1875000027312,43.6995308303616));
#9515=CARTESIAN_POINT('Ctrl Pts',(-105.5,43.1250000027312,0.));
#9516=CARTESIAN_POINT('Ctrl Pts',(-105.5,43.0625000027312,-43.6995308303615));
#9517=CARTESIAN_POINT('Ctrl Pts',(-74.5997654151808,43.0000000027312,-74.5997654151808));
#9518=CARTESIAN_POINT('Ctrl Pts',(-43.6995308303615,42.9375000027312,-105.5));
#9519=CARTESIAN_POINT('Ctrl Pts',(-6.46001186550229E-15,42.8750000027312,
-105.5));
#9520=CARTESIAN_POINT('Ctrl Pts',(43.6995308303615,42.8125000027312,-105.5));
#9521=CARTESIAN_POINT('Ctrl Pts',(74.5997654151808,42.7500000027312,-74.5997654151808));
#9522=CARTESIAN_POINT('Ctrl Pts',(105.5,42.6875000027312,-43.6995308303616));
#9523=CARTESIAN_POINT('Ctrl Pts',(105.5,42.6250000027312,-1.29200237310046E-14));
#9524=CARTESIAN_POINT('Ctrl Pts',(105.5,42.5625000027312,43.6995308303615));
#9525=CARTESIAN_POINT('Ctrl Pts',(74.5997654151808,42.5000000027312,74.5997654151808));
#9526=CARTESIAN_POINT('Ctrl Pts',(43.6995308303616,42.4375000027312,105.5));
#9527=CARTESIAN_POINT('Ctrl Pts',(1.93800355965069E-14,42.3750000027312,
105.5));
#9528=CARTESIAN_POINT('Ctrl Pts',(-43.6995308303616,42.3125000027312,105.5));
#9529=CARTESIAN_POINT('Ctrl Pts',(-74.5997654151808,42.2500000027312,74.5997654151808));
#9530=CARTESIAN_POINT('Ctrl Pts',(-105.5,42.1875000027312,43.6995308303616));
#9531=CARTESIAN_POINT('Ctrl Pts',(-105.5,42.1250000027312,0.));
#9532=CARTESIAN_POINT('Ctrl Pts',(-105.5,42.0625000027312,-43.6995308303615));
#9533=CARTESIAN_POINT('Ctrl Pts',(-74.5997654151808,42.0000000027312,-74.5997654151808));
#9534=CARTESIAN_POINT('Ctrl Pts',(-43.6995308303615,41.9375000027312,-105.5));
#9535=CARTESIAN_POINT('Ctrl Pts',(-6.46001186550229E-15,41.8750000027312,
-105.5));
#9536=CARTESIAN_POINT('Ctrl Pts',(43.6995308303615,41.8125000027312,-105.5));
#9537=CARTESIAN_POINT('Ctrl Pts',(74.5997654151808,41.7500000027312,-74.5997654151808));
#9538=CARTESIAN_POINT('Ctrl Pts',(105.5,41.6875000027312,-43.6995308303616));
#9539=CARTESIAN_POINT('Ctrl Pts',(105.5,41.6250000027312,-1.29200237310046E-14));
#9540=CARTESIAN_POINT('Ctrl Pts',(105.5,41.5625000027312,43.6995308303615));
#9541=CARTESIAN_POINT('Ctrl Pts',(74.5997654151808,41.5000000027312,74.5997654151808));
#9542=CARTESIAN_POINT('Ctrl Pts',(43.6995308303616,41.4375000027312,105.5));
#9543=CARTESIAN_POINT('Ctrl Pts',(1.93800355965069E-14,41.3750000027312,
105.5));
#9544=CARTESIAN_POINT('Ctrl Pts',(-43.6995308303616,41.3125000027312,105.5));
#9545=CARTESIAN_POINT('Ctrl Pts',(-74.5997654151808,41.2500000027312,74.5997654151808));
#9546=CARTESIAN_POINT('Ctrl Pts',(-105.5,41.1875000027312,43.6995308303616));
#9547=CARTESIAN_POINT('Ctrl Pts',(-105.5,41.1250000027312,0.));
#9548=CARTESIAN_POINT('Ctrl Pts',(-105.5,41.0625000027312,-43.6995308303615));
#9549=CARTESIAN_POINT('Ctrl Pts',(-74.5997654151808,41.0000000027312,-74.5997654151808));
#9550=CARTESIAN_POINT('Ctrl Pts',(-43.6995308303615,40.9375000027312,-105.5));
#9551=CARTESIAN_POINT('Ctrl Pts',(-6.46001186550229E-15,40.8750000027312,
-105.5));
#9552=CARTESIAN_POINT('Ctrl Pts',(43.6995308303615,40.8125000027312,-105.5));
#9553=CARTESIAN_POINT('Ctrl Pts',(74.5997654151808,40.7500000027312,-74.5997654151808));
#9554=CARTESIAN_POINT('Ctrl Pts',(105.5,40.6875000027312,-43.6995308303616));
#9555=CARTESIAN_POINT('Ctrl Pts',(105.5,40.6250000027312,-1.29200237310046E-14));
#9556=CARTESIAN_POINT('Ctrl Pts',(105.5,40.5625000027312,43.6995308303615));
#9557=CARTESIAN_POINT('Ctrl Pts',(74.5997654151808,40.5000000027312,74.5997654151808));
#9558=CARTESIAN_POINT('Ctrl Pts',(43.6995308303616,40.4375000027312,105.5));
#9559=CARTESIAN_POINT('Ctrl Pts',(1.93800355965069E-14,40.3750000027312,
105.5));
#9560=CARTESIAN_POINT('Ctrl Pts',(-43.6995308303616,40.3125000027312,105.5));
#9561=CARTESIAN_POINT('Ctrl Pts',(-74.5997654151808,40.2500000027312,74.5997654151808));
#9562=CARTESIAN_POINT('Ctrl Pts',(-105.5,40.1875000027312,43.6995308303616));
#9563=CARTESIAN_POINT('Ctrl Pts',(-105.5,40.1250000027312,0.));
#9564=CARTESIAN_POINT('Ctrl Pts',(-105.5,40.0625000027312,-43.6995308303615));
#9565=CARTESIAN_POINT('Ctrl Pts',(-74.5997654151808,40.0000000027312,-74.5997654151808));
#9566=CARTESIAN_POINT('Ctrl Pts',(-43.6995308303615,39.9375000027312,-105.5));
#9567=CARTESIAN_POINT('Ctrl Pts',(-6.46001186550229E-15,39.8750000027312,
-105.5));
#9568=CARTESIAN_POINT('Ctrl Pts',(43.6995308303615,39.8125000027312,-105.5));
#9569=CARTESIAN_POINT('Ctrl Pts',(74.5997654151808,39.7500000027312,-74.5997654151808));
#9570=CARTESIAN_POINT('Ctrl Pts',(105.5,39.6875000027312,-43.6995308303616));
#9571=CARTESIAN_POINT('Ctrl Pts',(105.5,39.6250000027312,-1.29200237310046E-14));
#9572=CARTESIAN_POINT('Ctrl Pts',(105.5,39.5625000027312,43.6995308303615));
#9573=CARTESIAN_POINT('Ctrl Pts',(74.5997654151808,39.5000000027312,74.5997654151808));
#9574=CARTESIAN_POINT('Ctrl Pts',(43.6995308303616,39.4375000027312,105.5));
#9575=CARTESIAN_POINT('Ctrl Pts',(1.93800355965069E-14,39.3750000027312,
105.5));
#9576=CARTESIAN_POINT('Ctrl Pts',(-43.6995308303616,39.3125000027312,105.5));
#9577=CARTESIAN_POINT('Ctrl Pts',(-74.5997654151808,39.2500000027312,74.5997654151808));
#9578=CARTESIAN_POINT('Ctrl Pts',(-105.5,39.1875000027312,43.6995308303616));
#9579=CARTESIAN_POINT('Ctrl Pts',(-105.5,39.1250000027312,0.));
#9580=CARTESIAN_POINT('Ctrl Pts',(-105.5,39.0625000027312,-43.6995308303615));
#9581=CARTESIAN_POINT('Ctrl Pts',(-74.5997654151808,39.0000000027312,-74.5997654151808));
#9582=CARTESIAN_POINT('Ctrl Pts',(-43.6995308303615,38.9375000027312,-105.5));
#9583=CARTESIAN_POINT('Ctrl Pts',(-6.46001186550229E-15,38.8750000027312,
-105.5));
#9584=CARTESIAN_POINT('Ctrl Pts',(43.6995308303615,38.8125000027312,-105.5));
#9585=CARTESIAN_POINT('Ctrl Pts',(74.5997654151808,38.7500000027312,-74.5997654151808));
#9586=CARTESIAN_POINT('Ctrl Pts',(105.5,38.6875000027312,-43.6995308303616));
#9587=CARTESIAN_POINT('Ctrl Pts',(105.5,38.6250000027312,-1.29200237310046E-14));
#9588=CARTESIAN_POINT('Ctrl Pts',(105.5,38.5625000027312,43.6995308303615));
#9589=CARTESIAN_POINT('Ctrl Pts',(74.5997654151808,38.5000000027312,74.5997654151808));
#9590=CARTESIAN_POINT('Ctrl Pts',(43.6995308303616,38.4375000027312,105.5));
#9591=CARTESIAN_POINT('Ctrl Pts',(1.93800355965069E-14,38.3750000027312,
105.5));
#9592=CARTESIAN_POINT('Ctrl Pts',(-43.6995308303616,38.3125000027312,105.5));
#9593=CARTESIAN_POINT('Ctrl Pts',(-74.5997654151808,38.2500000027312,74.5997654151808));
#9594=CARTESIAN_POINT('Ctrl Pts',(-105.5,38.1875000027312,43.6995308303616));
#9595=CARTESIAN_POINT('Ctrl Pts',(-105.5,38.1250000027312,0.));
#9596=CARTESIAN_POINT('Ctrl Pts',(-105.5,38.0625000027312,-43.6995308303615));
#9597=CARTESIAN_POINT('Ctrl Pts',(-74.5997654151808,38.0000000027312,-74.5997654151808));
#9598=CARTESIAN_POINT('Ctrl Pts',(-43.6995308303615,37.9375000027312,-105.5));
#9599=CARTESIAN_POINT('Ctrl Pts',(-6.46001186550229E-15,37.8750000027312,
-105.5));
#9600=CARTESIAN_POINT('Ctrl Pts',(43.6995308303615,37.8125000027312,-105.5));
#9601=CARTESIAN_POINT('Ctrl Pts',(74.5997654151808,37.7500000027312,-74.5997654151808));
#9602=CARTESIAN_POINT('Ctrl Pts',(105.5,37.6875000027312,-43.6995308303616));
#9603=CARTESIAN_POINT('Ctrl Pts',(105.5,37.6250000027312,-1.29200237310046E-14));
#9604=CARTESIAN_POINT('Ctrl Pts',(105.5,37.5625000027312,43.6995308303615));
#9605=CARTESIAN_POINT('Ctrl Pts',(74.5997654151808,37.5000000027312,74.5997654151808));
#9606=CARTESIAN_POINT('Ctrl Pts',(43.6995308303616,37.4375000027312,105.5));
#9607=CARTESIAN_POINT('Ctrl Pts',(1.93800355965069E-14,37.3750000027312,
105.5));
#9608=CARTESIAN_POINT('Ctrl Pts',(-43.6995308303616,37.3125000027312,105.5));
#9609=CARTESIAN_POINT('Ctrl Pts',(-74.5997654151808,37.2500000027312,74.5997654151808));
#9610=CARTESIAN_POINT('Ctrl Pts',(-105.5,37.1875000027312,43.6995308303616));
#9611=CARTESIAN_POINT('Ctrl Pts',(-105.5,37.1250000027312,0.));
#9612=CARTESIAN_POINT('Ctrl Pts',(-105.5,37.0625000027312,-43.6995308303615));
#9613=CARTESIAN_POINT('Ctrl Pts',(-74.5997654151808,37.0000000027312,-74.5997654151808));
#9614=CARTESIAN_POINT('Ctrl Pts',(-43.6995308303615,36.9375000027312,-105.5));
#9615=CARTESIAN_POINT('Ctrl Pts',(-6.46001186550229E-15,36.8750000027312,
-105.5));
#9616=CARTESIAN_POINT('Ctrl Pts',(43.6995308303615,36.8125000027312,-105.5));
#9617=CARTESIAN_POINT('Ctrl Pts',(74.5997654151808,36.7500000027312,-74.5997654151808));
#9618=CARTESIAN_POINT('Ctrl Pts',(105.5,36.6875000027312,-43.6995308303616));
#9619=CARTESIAN_POINT('Ctrl Pts',(105.5,36.6250000027312,-1.29200237310046E-14));
#9620=CARTESIAN_POINT('Ctrl Pts',(105.5,36.5625000027312,43.6995308303615));
#9621=CARTESIAN_POINT('Ctrl Pts',(74.5997654151808,36.5000000027312,74.5997654151808));
#9622=CARTESIAN_POINT('Ctrl Pts',(43.6995308303616,36.4375000027312,105.5));
#9623=CARTESIAN_POINT('Ctrl Pts',(1.93800355965069E-14,36.3750000027312,
105.5));
#9624=CARTESIAN_POINT('Ctrl Pts',(-43.6995308303616,36.3125000027312,105.5));
#9625=CARTESIAN_POINT('Ctrl Pts',(-74.5997654151808,36.2500000027312,74.5997654151808));
#9626=CARTESIAN_POINT('Ctrl Pts',(-105.5,36.1875000027312,43.6995308303616));
#9627=CARTESIAN_POINT('Ctrl Pts',(-105.5,36.1250000027312,0.));
#9628=CARTESIAN_POINT('Ctrl Pts',(-105.5,36.0625000027312,-43.6995308303615));
#9629=CARTESIAN_POINT('Ctrl Pts',(-74.5997654151808,36.0000000027312,-74.5997654151808));
#9630=CARTESIAN_POINT('Ctrl Pts',(-43.6995308303615,35.9375000027312,-105.5));
#9631=CARTESIAN_POINT('Ctrl Pts',(-6.46001186550229E-15,35.8750000027312,
-105.5));
#9632=CARTESIAN_POINT('Ctrl Pts',(43.6995308303615,35.8125000027312,-105.5));
#9633=CARTESIAN_POINT('Ctrl Pts',(74.5997654151808,35.7500000027312,-74.5997654151808));
#9634=CARTESIAN_POINT('Ctrl Pts',(105.5,35.6875000027312,-43.6995308303616));
#9635=CARTESIAN_POINT('Ctrl Pts',(105.5,35.6250000027312,-1.29200237310046E-14));
#9636=CARTESIAN_POINT('Ctrl Pts',(105.5,35.5625000027312,43.6995308303615));
#9637=CARTESIAN_POINT('Ctrl Pts',(74.5997654151808,35.5000000027312,74.5997654151808));
#9638=CARTESIAN_POINT('Ctrl Pts',(43.6995308303616,35.4375000027312,105.5));
#9639=CARTESIAN_POINT('Ctrl Pts',(1.93800355965069E-14,35.3750000027312,
105.5));
#9640=CARTESIAN_POINT('Ctrl Pts',(-43.6995308303616,35.3125000027312,105.5));
#9641=CARTESIAN_POINT('Ctrl Pts',(-74.5997654151808,35.2500000027312,74.5997654151808));
#9642=CARTESIAN_POINT('Ctrl Pts',(-105.5,35.1875000027312,43.6995308303616));
#9643=CARTESIAN_POINT('Ctrl Pts',(-105.5,35.1250000027312,0.));
#9644=CARTESIAN_POINT('Ctrl Pts',(-105.5,35.0625000027312,-43.6995308303615));
#9645=CARTESIAN_POINT('Ctrl Pts',(-74.5997654151808,35.0000000027312,-74.5997654151808));
#9646=CARTESIAN_POINT('Ctrl Pts',(-43.6995308303615,34.9375000027312,-105.5));
#9647=CARTESIAN_POINT('Ctrl Pts',(-6.46001186550229E-15,34.8750000027312,
-105.5));
#9648=CARTESIAN_POINT('Ctrl Pts',(43.6995308303615,34.8125000027312,-105.5));
#9649=CARTESIAN_POINT('Ctrl Pts',(74.5997654151808,34.7500000027312,-74.5997654151808));
#9650=CARTESIAN_POINT('Ctrl Pts',(105.5,34.6875000027312,-43.6995308303616));
#9651=CARTESIAN_POINT('Ctrl Pts',(105.5,34.6250000027312,-1.29200237310046E-14));
#9652=CARTESIAN_POINT('Ctrl Pts',(105.5,34.5625000027312,43.6995308303615));
#9653=CARTESIAN_POINT('Ctrl Pts',(74.5997654151808,34.5000000027312,74.5997654151808));
#9654=CARTESIAN_POINT('Ctrl Pts',(43.6995308303616,34.4375000027312,105.5));
#9655=CARTESIAN_POINT('Ctrl Pts',(1.93800355965069E-14,34.3750000027312,
105.5));
#9656=CARTESIAN_POINT('Ctrl Pts',(-43.6995308303616,34.3125000027312,105.5));
#9657=CARTESIAN_POINT('Ctrl Pts',(-74.5997654151808,34.2500000027312,74.5997654151808));
#9658=CARTESIAN_POINT('Ctrl Pts',(-105.5,34.1875000027312,43.6995308303616));
#9659=CARTESIAN_POINT('Ctrl Pts',(-105.5,34.1250000027312,0.));
#9660=CARTESIAN_POINT('Ctrl Pts',(-105.5,34.0625000027312,-43.6995308303615));
#9661=CARTESIAN_POINT('Ctrl Pts',(-74.5997654151808,34.0000000027312,-74.5997654151808));
#9662=CARTESIAN_POINT('Ctrl Pts',(-43.6995308303615,33.9375000027312,-105.5));
#9663=CARTESIAN_POINT('Ctrl Pts',(-6.46001186550229E-15,33.8750000027312,
-105.5));
#9664=CARTESIAN_POINT('Ctrl Pts',(43.6995308303615,33.8125000027312,-105.5));
#9665=CARTESIAN_POINT('Ctrl Pts',(74.5997654151808,33.7500000027312,-74.5997654151808));
#9666=CARTESIAN_POINT('Ctrl Pts',(105.5,33.6875000027312,-43.6995308303616));
#9667=CARTESIAN_POINT('Ctrl Pts',(105.5,33.6250000027312,-1.29200237310046E-14));
#9668=CARTESIAN_POINT('Ctrl Pts',(105.5,33.5625000027312,43.6995308303615));
#9669=CARTESIAN_POINT('Ctrl Pts',(74.5997654151808,33.5000000027312,74.5997654151808));
#9670=CARTESIAN_POINT('Ctrl Pts',(43.6995308303616,33.4375000027312,105.5));
#9671=CARTESIAN_POINT('Ctrl Pts',(1.93800355965069E-14,33.3750000027312,
105.5));
#9672=CARTESIAN_POINT('Ctrl Pts',(-43.6995308303616,33.3125000027312,105.5));
#9673=CARTESIAN_POINT('Ctrl Pts',(-74.5997654151808,33.2500000027312,74.5997654151808));
#9674=CARTESIAN_POINT('Ctrl Pts',(-105.5,33.1875000027312,43.6995308303616));
#9675=CARTESIAN_POINT('Ctrl Pts',(-105.5,33.1250000027312,0.));
#9676=CARTESIAN_POINT('Ctrl Pts',(-105.5,33.0625000027312,-43.6995308303615));
#9677=CARTESIAN_POINT('Ctrl Pts',(-74.5997654151808,33.0000000027312,-74.5997654151808));
#9678=CARTESIAN_POINT('Ctrl Pts',(-43.6995308303615,32.9375000027312,-105.5));
#9679=CARTESIAN_POINT('Ctrl Pts',(-6.46001186550229E-15,32.8750000027312,
-105.5));
#9680=CARTESIAN_POINT('Ctrl Pts',(43.6995308303615,32.8125000027312,-105.5));
#9681=CARTESIAN_POINT('Ctrl Pts',(74.5997654151808,32.7500000027312,-74.5997654151808));
#9682=CARTESIAN_POINT('Ctrl Pts',(105.5,32.6875000027312,-43.6995308303616));
#9683=CARTESIAN_POINT('Ctrl Pts',(105.5,32.6250000027312,-1.29200237310046E-14));
#9684=CARTESIAN_POINT('Ctrl Pts',(105.5,32.5625000027312,43.6995308303615));
#9685=CARTESIAN_POINT('Ctrl Pts',(74.5997654151808,32.5000000027312,74.5997654151808));
#9686=CARTESIAN_POINT('Ctrl Pts',(43.6995308303616,32.4375000027312,105.5));
#9687=CARTESIAN_POINT('Ctrl Pts',(1.93800355965069E-14,32.3750000027312,
105.5));
#9688=CARTESIAN_POINT('Ctrl Pts',(-43.6995308303616,32.3125000027312,105.5));
#9689=CARTESIAN_POINT('Ctrl Pts',(-74.5997654151808,32.2500000027312,74.5997654151808));
#9690=CARTESIAN_POINT('Ctrl Pts',(-105.5,32.1875000027312,43.6995308303616));
#9691=CARTESIAN_POINT('Ctrl Pts',(-105.5,32.1250000027312,0.));
#9692=CARTESIAN_POINT('Ctrl Pts',(-105.5,32.0625000027312,-43.6995308303615));
#9693=CARTESIAN_POINT('Ctrl Pts',(-74.5997654151808,32.0000000027312,-74.5997654151808));
#9694=CARTESIAN_POINT('Ctrl Pts',(-43.6995308303615,31.9375000027312,-105.5));
#9695=CARTESIAN_POINT('Ctrl Pts',(-6.46001186550229E-15,31.8750000027312,
-105.5));
#9696=CARTESIAN_POINT('Ctrl Pts',(43.6995308303615,31.8125000027312,-105.5));
#9697=CARTESIAN_POINT('Ctrl Pts',(74.5997654151808,31.7500000027312,-74.5997654151808));
#9698=CARTESIAN_POINT('Ctrl Pts',(105.5,31.6875000027312,-43.6995308303616));
#9699=CARTESIAN_POINT('Ctrl Pts',(105.5,31.6250000027312,-1.29200237310046E-14));
#9700=CARTESIAN_POINT('Ctrl Pts',(105.5,31.5625000027312,43.6995308303615));
#9701=CARTESIAN_POINT('Ctrl Pts',(74.5997654151808,31.5000000027312,74.5997654151808));
#9702=CARTESIAN_POINT('Ctrl Pts',(43.6995308303616,31.4375000027312,105.5));
#9703=CARTESIAN_POINT('Ctrl Pts',(1.93800355965069E-14,31.3750000027312,
105.5));
#9704=CARTESIAN_POINT('Ctrl Pts',(-43.6995308303616,31.3125000027312,105.5));
#9705=CARTESIAN_POINT('Ctrl Pts',(-74.5997654151808,31.2500000027312,74.5997654151808));
#9706=CARTESIAN_POINT('Ctrl Pts',(-105.5,31.1875000027312,43.6995308303616));
#9707=CARTESIAN_POINT('Ctrl Pts',(-105.5,31.1250000027312,0.));
#9708=CARTESIAN_POINT('Ctrl Pts',(-105.5,31.0625000027312,-43.6995308303615));
#9709=CARTESIAN_POINT('Ctrl Pts',(-74.5997654151808,31.0000000027312,-74.5997654151808));
#9710=CARTESIAN_POINT('Ctrl Pts',(-43.6995308303615,30.9375000027312,-105.5));
#9711=CARTESIAN_POINT('Ctrl Pts',(-6.46001186550229E-15,30.8750000027312,
-105.5));
#9712=CARTESIAN_POINT('Ctrl Pts',(43.6995308303615,30.8125000027312,-105.5));
#9713=CARTESIAN_POINT('Ctrl Pts',(74.5997654151808,30.7500000027312,-74.5997654151808));
#9714=CARTESIAN_POINT('Ctrl Pts',(105.5,30.6875000027312,-43.6995308303616));
#9715=CARTESIAN_POINT('Ctrl Pts',(105.5,30.6250000027312,-1.29200237310046E-14));
#9716=CARTESIAN_POINT('Ctrl Pts',(105.5,30.5625000027312,43.6995308303615));
#9717=CARTESIAN_POINT('Ctrl Pts',(74.5997654151808,30.5000000027312,74.5997654151808));
#9718=CARTESIAN_POINT('Ctrl Pts',(43.6995308303616,30.4375000027312,105.5));
#9719=CARTESIAN_POINT('Ctrl Pts',(1.93800355965069E-14,30.3750000027312,
105.5));
#9720=CARTESIAN_POINT('Ctrl Pts',(-43.6995308303616,30.3125000027312,105.5));
#9721=CARTESIAN_POINT('Ctrl Pts',(-74.5997654151808,30.2500000027312,74.5997654151808));
#9722=CARTESIAN_POINT('Ctrl Pts',(-105.5,30.1875000027312,43.6995308303616));
#9723=CARTESIAN_POINT('Ctrl Pts',(-105.5,30.1250000027312,0.));
#9724=CARTESIAN_POINT('Ctrl Pts',(-105.5,30.0625000027312,-43.6995308303615));
#9725=CARTESIAN_POINT('Ctrl Pts',(-74.5997654151808,30.0000000027312,-74.5997654151808));
#9726=CARTESIAN_POINT('Ctrl Pts',(-43.6995308303615,29.9375000027312,-105.5));
#9727=CARTESIAN_POINT('Ctrl Pts',(-6.46001186550229E-15,29.8750000027312,
-105.5));
#9728=CARTESIAN_POINT('Ctrl Pts',(43.6995308303615,29.8125000027312,-105.5));
#9729=CARTESIAN_POINT('Ctrl Pts',(74.5997654151808,29.7500000027312,-74.5997654151808));
#9730=CARTESIAN_POINT('Ctrl Pts',(105.5,29.6875000027312,-43.6995308303616));
#9731=CARTESIAN_POINT('Ctrl Pts',(105.5,29.6250000027312,-1.29200237310046E-14));
#9732=CARTESIAN_POINT('Ctrl Pts',(105.5,29.5625000027312,43.6995308303615));
#9733=CARTESIAN_POINT('Ctrl Pts',(74.5997654151808,29.5000000027312,74.5997654151808));
#9734=CARTESIAN_POINT('Ctrl Pts',(43.6995308303616,29.4375000027312,105.5));
#9735=CARTESIAN_POINT('Ctrl Pts',(1.93800355965069E-14,29.3750000027312,
105.5));
#9736=CARTESIAN_POINT('Ctrl Pts',(-43.6995308303616,29.3125000027312,105.5));
#9737=CARTESIAN_POINT('Ctrl Pts',(-74.5997654151808,29.2500000027312,74.5997654151808));
#9738=CARTESIAN_POINT('Ctrl Pts',(-105.5,29.1875000027312,43.6995308303616));
#9739=CARTESIAN_POINT('Ctrl Pts',(-105.5,29.1250000027312,0.));
#9740=CARTESIAN_POINT('Ctrl Pts',(-105.5,29.0625000027312,-43.6995308303615));
#9741=CARTESIAN_POINT('Ctrl Pts',(-74.5997654151808,29.0000000027312,-74.5997654151808));
#9742=CARTESIAN_POINT('Ctrl Pts',(-43.6995308303615,28.9375000027312,-105.5));
#9743=CARTESIAN_POINT('Ctrl Pts',(-6.46001186550229E-15,28.8750000027312,
-105.5));
#9744=CARTESIAN_POINT('Ctrl Pts',(43.6995308303615,28.8125000027312,-105.5));
#9745=CARTESIAN_POINT('Ctrl Pts',(74.5997654151808,28.7500000027312,-74.5997654151808));
#9746=CARTESIAN_POINT('Ctrl Pts',(105.5,28.6875000027312,-43.6995308303616));
#9747=CARTESIAN_POINT('Ctrl Pts',(105.5,28.6250000027312,-1.29200237310046E-14));
#9748=CARTESIAN_POINT('Ctrl Pts',(105.5,28.5625000027312,43.6995308303615));
#9749=CARTESIAN_POINT('Ctrl Pts',(74.5997654151808,28.5000000027312,74.5997654151808));
#9750=CARTESIAN_POINT('Ctrl Pts',(43.6995308303616,28.4375000027312,105.5));
#9751=CARTESIAN_POINT('Ctrl Pts',(1.93800355965069E-14,28.3750000027312,
105.5));
#9752=CARTESIAN_POINT('Ctrl Pts',(-43.6995308303616,28.3125000027312,105.5));
#9753=CARTESIAN_POINT('Ctrl Pts',(-74.5997654151808,28.2500000027312,74.5997654151808));
#9754=CARTESIAN_POINT('Ctrl Pts',(-105.5,28.1875000027312,43.6995308303616));
#9755=CARTESIAN_POINT('Ctrl Pts',(-105.5,28.1250000027312,0.));
#9756=CARTESIAN_POINT('Ctrl Pts',(-105.5,28.0625000027312,-43.6995308303615));
#9757=CARTESIAN_POINT('Ctrl Pts',(-74.5997654151808,28.0000000027312,-74.5997654151808));
#9758=CARTESIAN_POINT('Ctrl Pts',(-43.6995308303615,27.9375000027312,-105.5));
#9759=CARTESIAN_POINT('Ctrl Pts',(-6.46001186550229E-15,27.8750000027312,
-105.5));
#9760=CARTESIAN_POINT('Ctrl Pts',(43.6995308303615,27.8125000027312,-105.5));
#9761=CARTESIAN_POINT('Ctrl Pts',(74.5997654151808,27.7500000027312,-74.5997654151808));
#9762=CARTESIAN_POINT('Ctrl Pts',(105.5,27.6875000027312,-43.6995308303616));
#9763=CARTESIAN_POINT('Ctrl Pts',(105.5,27.6250000027312,-1.29200237310046E-14));
#9764=CARTESIAN_POINT('Ctrl Pts',(105.5,27.5625000027312,43.6995308303615));
#9765=CARTESIAN_POINT('Ctrl Pts',(74.5997654151808,27.5000000027312,74.5997654151808));
#9766=CARTESIAN_POINT('Ctrl Pts',(43.6995308303616,27.4375000027312,105.5));
#9767=CARTESIAN_POINT('Ctrl Pts',(1.93800355965069E-14,27.3750000027312,
105.5));
#9768=CARTESIAN_POINT('Ctrl Pts',(-43.6995308303616,27.3125000027312,105.5));
#9769=CARTESIAN_POINT('Ctrl Pts',(-74.5997654151808,27.2500000027312,74.5997654151808));
#9770=CARTESIAN_POINT('Ctrl Pts',(-105.5,27.1875000027312,43.6995308303616));
#9771=CARTESIAN_POINT('Ctrl Pts',(-105.5,27.1250000027312,0.));
#9772=CARTESIAN_POINT('Ctrl Pts',(-105.5,27.0625000027312,-43.6995308303615));
#9773=CARTESIAN_POINT('Ctrl Pts',(-74.5997654151808,27.0000000027312,-74.5997654151808));
#9774=CARTESIAN_POINT('Ctrl Pts',(-43.6995308303615,26.9375000027312,-105.5));
#9775=CARTESIAN_POINT('Ctrl Pts',(-6.46001186550229E-15,26.8750000027312,
-105.5));
#9776=CARTESIAN_POINT('Ctrl Pts',(43.6995308303615,26.8125000027312,-105.5));
#9777=CARTESIAN_POINT('Ctrl Pts',(74.5997654151808,26.7500000027312,-74.5997654151808));
#9778=CARTESIAN_POINT('Ctrl Pts',(105.5,26.6875000027312,-43.6995308303616));
#9779=CARTESIAN_POINT('Ctrl Pts',(105.5,26.6250000027312,-1.29200237310046E-14));
#9780=CARTESIAN_POINT('Ctrl Pts',(105.5,26.5625000027312,43.6995308303615));
#9781=CARTESIAN_POINT('Ctrl Pts',(74.5997654151808,26.5000000027312,74.5997654151808));
#9782=CARTESIAN_POINT('Ctrl Pts',(43.6995308303616,26.4375000027312,105.5));
#9783=CARTESIAN_POINT('Ctrl Pts',(1.93800355965069E-14,26.3750000027312,
105.5));
#9784=CARTESIAN_POINT('Ctrl Pts',(-43.6995308303616,26.3125000027312,105.5));
#9785=CARTESIAN_POINT('Ctrl Pts',(-74.5997654151808,26.2500000027312,74.5997654151808));
#9786=CARTESIAN_POINT('Ctrl Pts',(-105.5,26.1875000027312,43.6995308303616));
#9787=CARTESIAN_POINT('Ctrl Pts',(-105.5,26.1250000027312,0.));
#9788=CARTESIAN_POINT('Ctrl Pts',(-105.5,26.0625000027312,-43.6995308303615));
#9789=CARTESIAN_POINT('Ctrl Pts',(-74.5997654151808,26.0000000027312,-74.5997654151808));
#9790=CARTESIAN_POINT('Ctrl Pts',(-43.6995308303615,25.9375000027312,-105.5));
#9791=CARTESIAN_POINT('Ctrl Pts',(-6.46001186550229E-15,25.8750000027312,
-105.5));
#9792=CARTESIAN_POINT('Ctrl Pts',(43.6995308303615,25.8125000027312,-105.5));
#9793=CARTESIAN_POINT('Ctrl Pts',(74.5997654151808,25.7500000027312,-74.5997654151808));
#9794=CARTESIAN_POINT('Ctrl Pts',(105.5,25.6875000027312,-43.6995308303616));
#9795=CARTESIAN_POINT('Ctrl Pts',(105.5,25.6250000027312,-1.29200237310046E-14));
#9796=CARTESIAN_POINT('Ctrl Pts',(105.5,25.5625000027312,43.6995308303615));
#9797=CARTESIAN_POINT('Ctrl Pts',(74.5997654151808,25.5000000027312,74.5997654151808));
#9798=CARTESIAN_POINT('Ctrl Pts',(43.6995308303616,25.4375000027312,105.5));
#9799=CARTESIAN_POINT('Ctrl Pts',(1.93800355965069E-14,25.3750000027312,
105.5));
#9800=CARTESIAN_POINT('Ctrl Pts',(-43.6995308303616,25.3125000027312,105.5));
#9801=CARTESIAN_POINT('Ctrl Pts',(-74.5997654151808,25.2500000027312,74.5997654151808));
#9802=CARTESIAN_POINT('Ctrl Pts',(-105.5,25.1875000027312,43.6995308303616));
#9803=CARTESIAN_POINT('Ctrl Pts',(-105.5,25.1250000027312,0.));
#9804=CARTESIAN_POINT('Ctrl Pts',(-105.5,25.0625000027312,-43.6995308303615));
#9805=CARTESIAN_POINT('Ctrl Pts',(-74.5997654151808,25.0000000027312,-74.5997654151808));
#9806=CARTESIAN_POINT('Ctrl Pts',(-43.6995308303615,24.9375000027312,-105.5));
#9807=CARTESIAN_POINT('Ctrl Pts',(-6.46001186550229E-15,24.8750000027312,
-105.5));
#9808=CARTESIAN_POINT('Ctrl Pts',(43.6995308303615,24.8125000027312,-105.5));
#9809=CARTESIAN_POINT('Ctrl Pts',(74.5997654151808,24.7500000027312,-74.5997654151808));
#9810=CARTESIAN_POINT('Ctrl Pts',(105.5,24.6875000027312,-43.6995308303616));
#9811=CARTESIAN_POINT('Ctrl Pts',(105.5,24.6250000027312,-1.29200237310046E-14));
#9812=CARTESIAN_POINT('Ctrl Pts',(105.5,24.5625000027312,43.6995308303615));
#9813=CARTESIAN_POINT('Ctrl Pts',(74.5997654151808,24.5000000027312,74.5997654151808));
#9814=CARTESIAN_POINT('Ctrl Pts',(43.6995308303616,24.4375000027312,105.5));
#9815=CARTESIAN_POINT('Ctrl Pts',(1.93800355965069E-14,24.3750000027312,
105.5));
#9816=CARTESIAN_POINT('Ctrl Pts',(-43.6995308303616,24.3125000027312,105.5));
#9817=CARTESIAN_POINT('Ctrl Pts',(-74.5997654151808,24.2500000027312,74.5997654151808));
#9818=CARTESIAN_POINT('Ctrl Pts',(-105.5,24.1875000027312,43.6995308303616));
#9819=CARTESIAN_POINT('Ctrl Pts',(-105.5,24.1250000027312,0.));
#9820=CARTESIAN_POINT('Ctrl Pts',(-105.5,24.0625000027312,-43.6995308303615));
#9821=CARTESIAN_POINT('Ctrl Pts',(-74.5997654151808,24.0000000027312,-74.5997654151808));
#9822=CARTESIAN_POINT('Ctrl Pts',(-43.6995308303615,23.9375000027312,-105.5));
#9823=CARTESIAN_POINT('Ctrl Pts',(-6.46001186550229E-15,23.8750000027312,
-105.5));
#9824=CARTESIAN_POINT('Ctrl Pts',(43.6995308303615,23.8125000027312,-105.5));
#9825=CARTESIAN_POINT('Ctrl Pts',(74.5997654151808,23.7500000027312,-74.5997654151808));
#9826=CARTESIAN_POINT('Ctrl Pts',(105.5,23.6875000027312,-43.6995308303616));
#9827=CARTESIAN_POINT('Ctrl Pts',(105.5,23.6250000027312,-1.29200237310046E-14));
#9828=CARTESIAN_POINT('Ctrl Pts',(105.5,23.5625000027312,43.6995308303615));
#9829=CARTESIAN_POINT('Ctrl Pts',(74.5997654151808,23.5000000027312,74.5997654151808));
#9830=CARTESIAN_POINT('Ctrl Pts',(43.6995308303616,23.4375000027312,105.5));
#9831=CARTESIAN_POINT('Ctrl Pts',(1.93800355965069E-14,23.3750000027312,
105.5));
#9832=CARTESIAN_POINT('Ctrl Pts',(-43.6995308303616,23.3125000027312,105.5));
#9833=CARTESIAN_POINT('Ctrl Pts',(-74.5997654151808,23.2500000027312,74.5997654151808));
#9834=CARTESIAN_POINT('Ctrl Pts',(-105.5,23.1875000027312,43.6995308303616));
#9835=CARTESIAN_POINT('Ctrl Pts',(-105.5,23.1250000027312,0.));
#9836=CARTESIAN_POINT('Ctrl Pts',(-105.5,23.0625000027312,-43.6995308303615));
#9837=CARTESIAN_POINT('Ctrl Pts',(-74.5997654151808,23.0000000027312,-74.5997654151808));
#9838=CARTESIAN_POINT('Ctrl Pts',(-43.6995308303615,22.9375000027312,-105.5));
#9839=CARTESIAN_POINT('Ctrl Pts',(-6.46001186550229E-15,22.8750000027312,
-105.5));
#9840=CARTESIAN_POINT('Ctrl Pts',(43.6995308303615,22.8125000027312,-105.5));
#9841=CARTESIAN_POINT('Ctrl Pts',(74.5997654151808,22.7500000027312,-74.5997654151808));
#9842=CARTESIAN_POINT('Ctrl Pts',(105.5,22.6875000027312,-43.6995308303616));
#9843=CARTESIAN_POINT('Ctrl Pts',(105.5,22.6250000027312,-1.29200237310046E-14));
#9844=CARTESIAN_POINT('Ctrl Pts',(105.5,22.5625000027312,43.6995308303615));
#9845=CARTESIAN_POINT('Ctrl Pts',(74.5997654151808,22.5000000027312,74.5997654151808));
#9846=CARTESIAN_POINT('Ctrl Pts',(43.6995308303616,22.4375000027312,105.5));
#9847=CARTESIAN_POINT('Ctrl Pts',(1.93800355965069E-14,22.3750000027312,
105.5));
#9848=CARTESIAN_POINT('Ctrl Pts',(-43.6995308303616,22.3125000027312,105.5));
#9849=CARTESIAN_POINT('Ctrl Pts',(-74.5997654151808,22.2500000027312,74.5997654151808));
#9850=CARTESIAN_POINT('Ctrl Pts',(-105.5,22.1875000027312,43.6995308303616));
#9851=CARTESIAN_POINT('Ctrl Pts',(-105.5,22.1250000027312,0.));
#9852=CARTESIAN_POINT('Ctrl Pts',(-105.5,22.0625000027312,-43.6995308303615));
#9853=CARTESIAN_POINT('Ctrl Pts',(-74.5997654151808,22.0000000027312,-74.5997654151808));
#9854=CARTESIAN_POINT('Ctrl Pts',(-43.6995308303615,21.9375000027312,-105.5));
#9855=CARTESIAN_POINT('Ctrl Pts',(-6.46001186550229E-15,21.8750000027312,
-105.5));
#9856=CARTESIAN_POINT('Ctrl Pts',(43.6995308303615,21.8125000027312,-105.5));
#9857=CARTESIAN_POINT('Ctrl Pts',(74.5997654151808,21.7500000027312,-74.5997654151808));
#9858=CARTESIAN_POINT('Ctrl Pts',(105.5,21.6875000027312,-43.6995308303616));
#9859=CARTESIAN_POINT('Ctrl Pts',(105.5,21.6250000027312,-1.29200237310046E-14));
#9860=CARTESIAN_POINT('Ctrl Pts',(105.5,21.5625000027312,43.6995308303615));
#9861=CARTESIAN_POINT('Ctrl Pts',(74.5997654151808,21.5000000027312,74.5997654151808));
#9862=CARTESIAN_POINT('Ctrl Pts',(43.6995308303616,21.4375000027312,105.5));
#9863=CARTESIAN_POINT('Ctrl Pts',(1.93800355965069E-14,21.3750000027312,
105.5));
#9864=CARTESIAN_POINT('Ctrl Pts',(-43.6995308303616,21.3125000027312,105.5));
#9865=CARTESIAN_POINT('Ctrl Pts',(-74.5997654151808,21.2500000027312,74.5997654151808));
#9866=CARTESIAN_POINT('Ctrl Pts',(-105.5,21.1875000027312,43.6995308303616));
#9867=CARTESIAN_POINT('Ctrl Pts',(-105.5,21.1250000027312,0.));
#9868=CARTESIAN_POINT('Ctrl Pts',(-105.5,21.0625000027312,-43.6995308303615));
#9869=CARTESIAN_POINT('Ctrl Pts',(-74.5997654151808,21.0000000027312,-74.5997654151808));
#9870=CARTESIAN_POINT('Ctrl Pts',(-43.6995308303615,20.9375000027312,-105.5));
#9871=CARTESIAN_POINT('Ctrl Pts',(-6.46001186550229E-15,20.8750000027312,
-105.5));
#9872=CARTESIAN_POINT('Ctrl Pts',(43.6995308303615,20.8125000027312,-105.5));
#9873=CARTESIAN_POINT('Ctrl Pts',(74.5997654151808,20.7500000027312,-74.5997654151808));
#9874=CARTESIAN_POINT('Ctrl Pts',(105.5,20.6875000027312,-43.6995308303616));
#9875=CARTESIAN_POINT('Ctrl Pts',(105.5,20.6250000027312,-1.29200237310046E-14));
#9876=CARTESIAN_POINT('Ctrl Pts',(105.5,20.5625000027312,43.6995308303615));
#9877=CARTESIAN_POINT('Ctrl Pts',(74.5997654151808,20.5000000027312,74.5997654151808));
#9878=CARTESIAN_POINT('Ctrl Pts',(43.6995308303616,20.4375000027312,105.5));
#9879=CARTESIAN_POINT('Ctrl Pts',(1.93800355965069E-14,20.3750000027312,
105.5));
#9880=CARTESIAN_POINT('Ctrl Pts',(-43.6995308303616,20.3125000027312,105.5));
#9881=CARTESIAN_POINT('Ctrl Pts',(-74.5997654151808,20.2500000027312,74.5997654151808));
#9882=CARTESIAN_POINT('Ctrl Pts',(-105.5,20.1875000027312,43.6995308303616));
#9883=CARTESIAN_POINT('Ctrl Pts',(-105.5,20.1250000027312,0.));
#9884=CARTESIAN_POINT('Ctrl Pts',(-105.5,20.0625000027312,-43.6995308303615));
#9885=CARTESIAN_POINT('Ctrl Pts',(-74.5997654151808,20.0000000027312,-74.5997654151808));
#9886=CARTESIAN_POINT('Ctrl Pts',(-43.6995308303615,19.9375000027312,-105.5));
#9887=CARTESIAN_POINT('Ctrl Pts',(-6.46001186550229E-15,19.8750000027312,
-105.5));
#9888=CARTESIAN_POINT('Ctrl Pts',(43.6995308303615,19.8125000027312,-105.5));
#9889=CARTESIAN_POINT('Ctrl Pts',(74.5997654151808,19.7500000027312,-74.5997654151808));
#9890=CARTESIAN_POINT('Ctrl Pts',(105.5,19.6875000027312,-43.6995308303616));
#9891=CARTESIAN_POINT('Ctrl Pts',(105.5,19.6250000027312,-1.29200237310046E-14));
#9892=CARTESIAN_POINT('Ctrl Pts',(105.5,19.5625000027312,43.6995308303615));
#9893=CARTESIAN_POINT('Ctrl Pts',(74.5997654151808,19.5000000027312,74.5997654151808));
#9894=CARTESIAN_POINT('Ctrl Pts',(43.6995308303616,19.4375000027312,105.5));
#9895=CARTESIAN_POINT('Ctrl Pts',(1.93800355965069E-14,19.3750000027312,
105.5));
#9896=CARTESIAN_POINT('Ctrl Pts',(-43.6995308303616,19.3125000027312,105.5));
#9897=CARTESIAN_POINT('Ctrl Pts',(-74.5997654151808,19.2500000027312,74.5997654151808));
#9898=CARTESIAN_POINT('Ctrl Pts',(-105.5,19.1875000027312,43.6995308303616));
#9899=CARTESIAN_POINT('Ctrl Pts',(-105.5,19.1250000027312,0.));
#9900=CARTESIAN_POINT('Ctrl Pts',(-105.5,19.0625000027312,-43.6995308303615));
#9901=CARTESIAN_POINT('Ctrl Pts',(-74.5997654151808,19.0000000027312,-74.5997654151808));
#9902=CARTESIAN_POINT('Ctrl Pts',(-43.6995308303615,18.9375000027312,-105.5));
#9903=CARTESIAN_POINT('Ctrl Pts',(-6.46001186550229E-15,18.8750000027312,
-105.5));
#9904=CARTESIAN_POINT('Ctrl Pts',(43.6995308303615,18.8125000027312,-105.5));
#9905=CARTESIAN_POINT('Ctrl Pts',(74.5997654151808,18.7500000027312,-74.5997654151808));
#9906=CARTESIAN_POINT('Ctrl Pts',(105.5,18.6875000027312,-43.6995308303616));
#9907=CARTESIAN_POINT('Ctrl Pts',(105.5,18.6250000027312,-1.29200237310046E-14));
#9908=CARTESIAN_POINT('Ctrl Pts',(105.5,18.5625000027312,43.6995308303615));
#9909=CARTESIAN_POINT('Ctrl Pts',(74.5997654151808,18.5000000027312,74.5997654151808));
#9910=CARTESIAN_POINT('Ctrl Pts',(43.6995308303616,18.4375000027312,105.5));
#9911=CARTESIAN_POINT('Ctrl Pts',(1.93800355965069E-14,18.3750000027312,
105.5));
#9912=CARTESIAN_POINT('Ctrl Pts',(-43.6995308303616,18.3125000027312,105.5));
#9913=CARTESIAN_POINT('Ctrl Pts',(-74.5997654151808,18.2500000027312,74.5997654151808));
#9914=CARTESIAN_POINT('Ctrl Pts',(-105.5,18.1875000027312,43.6995308303616));
#9915=CARTESIAN_POINT('Ctrl Pts',(-105.5,18.1250000027312,0.));
#9916=CARTESIAN_POINT('Ctrl Pts',(-105.5,18.0625000027312,-43.6995308303615));
#9917=CARTESIAN_POINT('Ctrl Pts',(-74.5997654151808,18.0000000027312,-74.5997654151808));
#9918=CARTESIAN_POINT('Ctrl Pts',(-43.6995308303615,17.9375000027312,-105.5));
#9919=CARTESIAN_POINT('Ctrl Pts',(-6.46001186550229E-15,17.8750000027312,
-105.5));
#9920=CARTESIAN_POINT('Ctrl Pts',(43.6995308303615,17.8125000027312,-105.5));
#9921=CARTESIAN_POINT('Ctrl Pts',(74.5997654151808,17.7500000027312,-74.5997654151808));
#9922=CARTESIAN_POINT('Ctrl Pts',(105.5,17.6875000027312,-43.6995308303616));
#9923=CARTESIAN_POINT('Ctrl Pts',(105.5,17.6250000027312,-1.29200237310046E-14));
#9924=CARTESIAN_POINT('Ctrl Pts',(105.5,17.5625000027312,43.6995308303615));
#9925=CARTESIAN_POINT('Ctrl Pts',(74.5997654151808,17.5000000027312,74.5997654151808));
#9926=CARTESIAN_POINT('Ctrl Pts',(43.6995308303616,17.4375000027312,105.5));
#9927=CARTESIAN_POINT('Ctrl Pts',(1.93800355965069E-14,17.3750000027312,
105.5));
#9928=CARTESIAN_POINT('Ctrl Pts',(-43.6995308303616,17.3125000027312,105.5));
#9929=CARTESIAN_POINT('Ctrl Pts',(-74.5997654151808,17.2500000027312,74.5997654151808));
#9930=CARTESIAN_POINT('Ctrl Pts',(-105.5,17.1875000027312,43.6995308303616));
#9931=CARTESIAN_POINT('Ctrl Pts',(-105.5,17.1250000027312,0.));
#9932=CARTESIAN_POINT('Ctrl Pts',(-105.5,17.0625000027312,-43.6995308303615));
#9933=CARTESIAN_POINT('Ctrl Pts',(-74.5997654151808,17.0000000027312,-74.5997654151808));
#9934=CARTESIAN_POINT('Ctrl Pts',(-43.6995308303615,16.9375000027312,-105.5));
#9935=CARTESIAN_POINT('Ctrl Pts',(-6.46001186550229E-15,16.8750000027312,
-105.5));
#9936=CARTESIAN_POINT('Ctrl Pts',(43.6995308303615,16.8125000027312,-105.5));
#9937=CARTESIAN_POINT('Ctrl Pts',(74.5997654151808,16.7500000027312,-74.5997654151808));
#9938=CARTESIAN_POINT('Ctrl Pts',(105.5,16.6875000027312,-43.6995308303616));
#9939=CARTESIAN_POINT('Ctrl Pts',(105.5,16.6250000027312,-1.29200237310046E-14));
#9940=CARTESIAN_POINT('Ctrl Pts',(105.5,16.5625000027312,43.6995308303615));
#9941=CARTESIAN_POINT('Ctrl Pts',(74.5997654151808,16.5000000027312,74.5997654151808));
#9942=CARTESIAN_POINT('Ctrl Pts',(43.6995308303616,16.4375000027312,105.5));
#9943=CARTESIAN_POINT('Ctrl Pts',(1.93800355965069E-14,16.3750000027312,
105.5));
#9944=CARTESIAN_POINT('Ctrl Pts',(-43.6995308303616,16.3125000027312,105.5));
#9945=CARTESIAN_POINT('Ctrl Pts',(-74.5997654151808,16.2500000027312,74.5997654151808));
#9946=CARTESIAN_POINT('Ctrl Pts',(-105.5,16.1875000027312,43.6995308303616));
#9947=CARTESIAN_POINT('Ctrl Pts',(-105.5,16.1250000027312,0.));
#9948=CARTESIAN_POINT('Ctrl Pts',(-105.5,16.0625000027312,-43.6995308303615));
#9949=CARTESIAN_POINT('Ctrl Pts',(-74.5997654151808,16.0000000027312,-74.5997654151808));
#9950=CARTESIAN_POINT('Ctrl Pts',(-43.6995308303615,15.9375000027312,-105.5));
#9951=CARTESIAN_POINT('Ctrl Pts',(-6.46001186550229E-15,15.8750000027312,
-105.5));
#9952=CARTESIAN_POINT('Ctrl Pts',(43.6995308303615,15.8125000027312,-105.5));
#9953=CARTESIAN_POINT('Ctrl Pts',(74.5997654151808,15.7500000027312,-74.5997654151808));
#9954=CARTESIAN_POINT('Ctrl Pts',(105.5,15.6875000027312,-43.6995308303616));
#9955=CARTESIAN_POINT('Ctrl Pts',(105.5,15.6250000027312,-1.29200237310046E-14));
#9956=CARTESIAN_POINT('Ctrl Pts',(105.5,15.5625000027312,43.6995308303615));
#9957=CARTESIAN_POINT('Ctrl Pts',(74.5997654151808,15.5000000027312,74.5997654151808));
#9958=CARTESIAN_POINT('Ctrl Pts',(43.6995308303616,15.4375000027312,105.5));
#9959=CARTESIAN_POINT('Ctrl Pts',(1.93800355965069E-14,15.3750000027312,
105.5));
#9960=CARTESIAN_POINT('Ctrl Pts',(-43.6995308303616,15.3125000027312,105.5));
#9961=CARTESIAN_POINT('Ctrl Pts',(-74.5997654151808,15.2500000027312,74.5997654151808));
#9962=CARTESIAN_POINT('Ctrl Pts',(-105.5,15.1875000027312,43.6995308303616));
#9963=CARTESIAN_POINT('Ctrl Pts',(-105.5,15.1250000027312,0.));
#9964=CARTESIAN_POINT('Ctrl Pts',(-105.5,15.0625000027312,-43.6995308303615));
#9965=CARTESIAN_POINT('Ctrl Pts',(-74.5997654151808,15.0000000027312,-74.5997654151808));
#9966=CARTESIAN_POINT('Ctrl Pts',(-43.6995308303615,14.9375000027312,-105.5));
#9967=CARTESIAN_POINT('Ctrl Pts',(-6.46001186550229E-15,14.8750000027312,
-105.5));
#9968=CARTESIAN_POINT('Ctrl Pts',(43.6995308303615,14.8125000027312,-105.5));
#9969=CARTESIAN_POINT('Ctrl Pts',(74.5997654151808,14.7500000027312,-74.5997654151808));
#9970=CARTESIAN_POINT('Ctrl Pts',(105.5,14.6875000027312,-43.6995308303616));
#9971=CARTESIAN_POINT('Ctrl Pts',(105.5,14.6250000027312,-1.29200237310046E-14));
#9972=CARTESIAN_POINT('Ctrl Pts',(105.5,14.5625000027312,43.6995308303615));
#9973=CARTESIAN_POINT('Ctrl Pts',(74.5997654151808,14.5000000027312,74.5997654151808));
#9974=CARTESIAN_POINT('Ctrl Pts',(43.6995308303616,14.4375000027312,105.5));
#9975=CARTESIAN_POINT('Ctrl Pts',(1.93800355965069E-14,14.3750000027312,
105.5));
#9976=CARTESIAN_POINT('Ctrl Pts',(-43.6995308303616,14.3125000027312,105.5));
#9977=CARTESIAN_POINT('Ctrl Pts',(-74.5997654151808,14.2500000027312,74.5997654151808));
#9978=CARTESIAN_POINT('Ctrl Pts',(-105.5,14.1875000027312,43.6995308303616));
#9979=CARTESIAN_POINT('Ctrl Pts',(-105.5,14.1250000027312,0.));
#9980=CARTESIAN_POINT('Ctrl Pts',(-105.5,14.0625000027312,-43.6995308303615));
#9981=CARTESIAN_POINT('Ctrl Pts',(-74.5997654151808,14.0000000027312,-74.5997654151808));
#9982=CARTESIAN_POINT('Ctrl Pts',(-43.6995308303615,13.9375000027312,-105.5));
#9983=CARTESIAN_POINT('Ctrl Pts',(-6.46001186550229E-15,13.8750000027312,
-105.5));
#9984=CARTESIAN_POINT('Ctrl Pts',(43.6995308303615,13.8125000027312,-105.5));
#9985=CARTESIAN_POINT('Ctrl Pts',(74.5997654151808,13.7500000027312,-74.5997654151808));
#9986=CARTESIAN_POINT('Ctrl Pts',(105.5,13.6875000027312,-43.6995308303616));
#9987=CARTESIAN_POINT('Ctrl Pts',(105.5,13.6250000027312,-1.29200237310046E-14));
#9988=CARTESIAN_POINT('Ctrl Pts',(105.5,13.5625000027312,43.6995308303615));
#9989=CARTESIAN_POINT('Ctrl Pts',(74.5997654151808,13.5000000027312,74.5997654151808));
#9990=CARTESIAN_POINT('Ctrl Pts',(43.6995308303616,13.4375000027312,105.5));
#9991=CARTESIAN_POINT('Ctrl Pts',(1.93800355965069E-14,13.3750000027312,
105.5));
#9992=CARTESIAN_POINT('Ctrl Pts',(-43.6995308303616,13.3125000027312,105.5));
#9993=CARTESIAN_POINT('Ctrl Pts',(-74.5997654151808,13.2500000027312,74.5997654151808));
#9994=CARTESIAN_POINT('Ctrl Pts',(-105.5,13.1875000027312,43.6995308303616));
#9995=CARTESIAN_POINT('Ctrl Pts',(-105.5,13.1250000027312,0.));
#9996=CARTESIAN_POINT('Ctrl Pts',(-105.5,13.0625000027312,-43.6995308303615));
#9997=CARTESIAN_POINT('Ctrl Pts',(-74.5997654151808,13.0000000027312,-74.5997654151808));
#9998=CARTESIAN_POINT('Ctrl Pts',(-43.6995308303615,12.9375000027312,-105.5));
#9999=CARTESIAN_POINT('Ctrl Pts',(-6.46001186550229E-15,12.8750000027312,
-105.5));
#10000=CARTESIAN_POINT('Ctrl Pts',(43.6995308303615,12.8125000027312,-105.5));
#10001=CARTESIAN_POINT('Ctrl Pts',(74.5997654151808,12.7500000027312,-74.5997654151808));
#10002=CARTESIAN_POINT('Ctrl Pts',(105.5,12.6875000027312,-43.6995308303616));
#10003=CARTESIAN_POINT('Ctrl Pts',(105.5,12.6250000027312,-1.29200237310046E-14));
#10004=CARTESIAN_POINT('Ctrl Pts',(105.5,12.5625000027312,43.6995308303615));
#10005=CARTESIAN_POINT('Ctrl Pts',(74.5997654151808,12.5000000027312,74.5997654151808));
#10006=CARTESIAN_POINT('Ctrl Pts',(43.6995308303616,12.4375000027312,105.5));
#10007=CARTESIAN_POINT('Ctrl Pts',(1.93800355965069E-14,12.3750000027312,
105.5));
#10008=CARTESIAN_POINT('Ctrl Pts',(-43.6995308303616,12.3125000027312,105.5));
#10009=CARTESIAN_POINT('Ctrl Pts',(-74.5997654151808,12.2500000027312,74.5997654151808));
#10010=CARTESIAN_POINT('Ctrl Pts',(-105.5,12.1875000027312,43.6995308303616));
#10011=CARTESIAN_POINT('Ctrl Pts',(-105.5,12.1250000027312,0.));
#10012=CARTESIAN_POINT('Ctrl Pts',(-105.5,12.0625000027312,-43.6995308303615));
#10013=CARTESIAN_POINT('Ctrl Pts',(-74.5997654151808,12.0000000027312,-74.5997654151808));
#10014=CARTESIAN_POINT('Ctrl Pts',(-43.6995308303615,11.9375000027312,-105.5));
#10015=CARTESIAN_POINT('Ctrl Pts',(-6.46001186550229E-15,11.8750000027312,
-105.5));
#10016=CARTESIAN_POINT('Ctrl Pts',(43.6995308303615,11.8125000027312,-105.5));
#10017=CARTESIAN_POINT('Ctrl Pts',(74.5997654151808,11.7500000027312,-74.5997654151808));
#10018=CARTESIAN_POINT('Ctrl Pts',(105.5,11.6875000027312,-43.6995308303616));
#10019=CARTESIAN_POINT('Ctrl Pts',(105.5,11.6250000027312,-1.29200237310046E-14));
#10020=CARTESIAN_POINT('Ctrl Pts',(105.5,11.5625000027312,43.6995308303615));
#10021=CARTESIAN_POINT('Ctrl Pts',(74.5997654151808,11.5000000027312,74.5997654151808));
#10022=CARTESIAN_POINT('Ctrl Pts',(43.6995308303616,11.4375000027312,105.5));
#10023=CARTESIAN_POINT('Ctrl Pts',(1.93800355965069E-14,11.3750000027312,
105.5));
#10024=CARTESIAN_POINT('Ctrl Pts',(-43.6995308303616,11.3125000027312,105.5));
#10025=CARTESIAN_POINT('Ctrl Pts',(-74.5997654151808,11.2500000027312,74.5997654151808));
#10026=CARTESIAN_POINT('Ctrl Pts',(-105.5,11.1875000027312,43.6995308303616));
#10027=CARTESIAN_POINT('Ctrl Pts',(-105.5,11.1250000027312,0.));
#10028=CARTESIAN_POINT('Ctrl Pts',(-105.5,11.0625000027312,-43.6995308303615));
#10029=CARTESIAN_POINT('Ctrl Pts',(-74.5997654151808,11.0000000027312,-74.5997654151808));
#10030=CARTESIAN_POINT('Ctrl Pts',(-43.6995308303615,10.9375000027312,-105.5));
#10031=CARTESIAN_POINT('Ctrl Pts',(-6.46001186550229E-15,10.8750000027312,
-105.5));
#10032=CARTESIAN_POINT('Ctrl Pts',(43.6995308303615,10.8125000027312,-105.5));
#10033=CARTESIAN_POINT('Ctrl Pts',(74.5997654151808,10.7500000027312,-74.5997654151808));
#10034=CARTESIAN_POINT('Ctrl Pts',(105.5,10.6875000027312,-43.6995308303616));
#10035=CARTESIAN_POINT('Ctrl Pts',(105.5,10.6250000027312,-1.29200237310046E-14));
#10036=CARTESIAN_POINT('Ctrl Pts',(105.5,10.5625000027312,43.6995308303615));
#10037=CARTESIAN_POINT('Ctrl Pts',(74.5997654151808,10.5000000027312,74.5997654151808));
#10038=CARTESIAN_POINT('Ctrl Pts',(43.6995308303616,10.4375000027312,105.5));
#10039=CARTESIAN_POINT('Ctrl Pts',(1.93800355965069E-14,10.3750000027312,
105.5));
#10040=CARTESIAN_POINT('Ctrl Pts',(-43.6995308303616,10.3125000027312,105.5));
#10041=CARTESIAN_POINT('Ctrl Pts',(-74.5997654151808,10.2500000027312,74.5997654151808));
#10042=CARTESIAN_POINT('Ctrl Pts',(-105.5,10.1875000027312,43.6995308303616));
#10043=CARTESIAN_POINT('Ctrl Pts',(-105.5,10.1250000027312,0.));
#10044=CARTESIAN_POINT('Ctrl Pts',(-105.5,10.0625000027312,-43.6995308303615));
#10045=CARTESIAN_POINT('Ctrl Pts',(-74.5997654151808,10.0000000027312,-74.5997654151808));
#10046=CARTESIAN_POINT('Ctrl Pts',(-43.6995308303615,9.93750000273118,-105.5));
#10047=CARTESIAN_POINT('Ctrl Pts',(-6.46001186550229E-15,9.87500000273118,
-105.5));
#10048=CARTESIAN_POINT('Ctrl Pts',(43.6995308303615,9.81250000273118,-105.5));
#10049=CARTESIAN_POINT('Ctrl Pts',(74.5997654151808,9.75000000273118,-74.5997654151808));
#10050=CARTESIAN_POINT('Ctrl Pts',(105.5,9.68750000273118,-43.6995308303616));
#10051=CARTESIAN_POINT('Ctrl Pts',(105.5,9.62500000273118,-1.29200237310046E-14));
#10052=CARTESIAN_POINT('Ctrl Pts',(105.5,9.56250000273118,43.6995308303615));
#10053=CARTESIAN_POINT('Ctrl Pts',(74.5997654151808,9.50000000273118,74.5997654151808));
#10054=CARTESIAN_POINT('Ctrl Pts',(43.6995308303616,9.43750000273118,105.5));
#10055=CARTESIAN_POINT('Ctrl Pts',(1.93800355965069E-14,9.37500000273118,
105.5));
#10056=CARTESIAN_POINT('Ctrl Pts',(-43.6995308303616,9.31250000273118,105.5));
#10057=CARTESIAN_POINT('Ctrl Pts',(-74.5997654151808,9.25000000273118,74.5997654151808));
#10058=CARTESIAN_POINT('Ctrl Pts',(-105.5,9.18750000273118,43.6995308303616));
#10059=CARTESIAN_POINT('Ctrl Pts',(-105.5,9.12500000273118,0.));
#10060=CARTESIAN_POINT('Ctrl Pts',(-105.5,9.06250000273118,-43.6995308303615));
#10061=CARTESIAN_POINT('Ctrl Pts',(-74.5997654151808,9.00000000273118,-74.5997654151808));
#10062=CARTESIAN_POINT('Ctrl Pts',(-43.6995308303615,8.93750000273118,-105.5));
#10063=CARTESIAN_POINT('Ctrl Pts',(-6.46001186550229E-15,8.87500000273118,
-105.5));
#10064=CARTESIAN_POINT('Ctrl Pts',(43.6995308303615,8.81250000273118,-105.5));
#10065=CARTESIAN_POINT('Ctrl Pts',(74.5997654151808,8.75000000273118,-74.5997654151808));
#10066=CARTESIAN_POINT('Ctrl Pts',(105.5,8.68750000273118,-43.6995308303616));
#10067=CARTESIAN_POINT('Ctrl Pts',(105.5,8.62500000273118,-1.29200237310046E-14));
#10068=CARTESIAN_POINT('Ctrl Pts',(105.5,8.56250000273118,43.6995308303615));
#10069=CARTESIAN_POINT('Ctrl Pts',(74.5997654151808,8.50000000273118,74.5997654151808));
#10070=CARTESIAN_POINT('Ctrl Pts',(43.6995308303616,8.43750000273118,105.5));
#10071=CARTESIAN_POINT('Ctrl Pts',(1.93800355965069E-14,8.37500000273118,
105.5));
#10072=CARTESIAN_POINT('Ctrl Pts',(-43.6995308303616,8.31250000273118,105.5));
#10073=CARTESIAN_POINT('Ctrl Pts',(-74.5997654151808,8.25000000273118,74.5997654151808));
#10074=CARTESIAN_POINT('Ctrl Pts',(-105.5,8.18750000273118,43.6995308303616));
#10075=CARTESIAN_POINT('Ctrl Pts',(-105.5,8.12500000273118,0.));
#10076=CARTESIAN_POINT('Ctrl Pts',(-105.5,8.06250000273118,-43.6995308303615));
#10077=CARTESIAN_POINT('Ctrl Pts',(-74.5997654151808,8.00000000273118,-74.5997654151808));
#10078=CARTESIAN_POINT('Ctrl Pts',(-43.6995308303615,7.93750000273118,-105.5));
#10079=CARTESIAN_POINT('Ctrl Pts',(-6.46001186550229E-15,7.87500000273118,
-105.5));
#10080=CARTESIAN_POINT('Ctrl Pts',(43.6995308303615,7.81250000273118,-105.5));
#10081=CARTESIAN_POINT('Ctrl Pts',(74.5997654151808,7.75000000273118,-74.5997654151808));
#10082=CARTESIAN_POINT('Ctrl Pts',(105.5,7.68750000273118,-43.6995308303616));
#10083=CARTESIAN_POINT('Ctrl Pts',(105.5,7.62500000273118,-1.29200237310046E-14));
#10084=CARTESIAN_POINT('Ctrl Pts',(105.5,7.56250000273118,43.6995308303615));
#10085=CARTESIAN_POINT('Ctrl Pts',(74.5997654151808,7.50000000273118,74.5997654151808));
#10086=CARTESIAN_POINT('Ctrl Pts',(43.6995308303616,7.43750000273118,105.5));
#10087=CARTESIAN_POINT('Ctrl Pts',(1.93800355965069E-14,7.37500000273118,
105.5));
#10088=CARTESIAN_POINT('Ctrl Pts',(-43.6995308303616,7.31250000273118,105.5));
#10089=CARTESIAN_POINT('Ctrl Pts',(-74.5997654151808,7.25000000273118,74.5997654151808));
#10090=CARTESIAN_POINT('Ctrl Pts',(-105.5,7.18750000273118,43.6995308303616));
#10091=CARTESIAN_POINT('Ctrl Pts',(-105.5,7.12500000273118,0.));
#10092=CARTESIAN_POINT('Ctrl Pts',(-105.5,7.06250000273118,-43.6995308303615));
#10093=CARTESIAN_POINT('Ctrl Pts',(-74.5997654151808,7.00000000273118,-74.5997654151808));
#10094=CARTESIAN_POINT('Ctrl Pts',(-43.6995308303615,6.93750000273118,-105.5));
#10095=CARTESIAN_POINT('Ctrl Pts',(-6.46001186550229E-15,6.87500000273118,
-105.5));
#10096=CARTESIAN_POINT('Ctrl Pts',(43.6995308303615,6.81250000273118,-105.5));
#10097=CARTESIAN_POINT('Ctrl Pts',(74.5997654151808,6.75000000273118,-74.5997654151808));
#10098=CARTESIAN_POINT('Ctrl Pts',(105.5,6.68750000273118,-43.6995308303616));
#10099=CARTESIAN_POINT('Ctrl Pts',(105.5,6.62500000273118,-1.29200237310046E-14));
#10100=CARTESIAN_POINT('Ctrl Pts',(105.5,6.56250000273118,43.6995308303615));
#10101=CARTESIAN_POINT('Ctrl Pts',(74.5997654151808,6.50000000273118,74.5997654151808));
#10102=CARTESIAN_POINT('Ctrl Pts',(43.6995308303616,6.43750000273118,105.5));
#10103=CARTESIAN_POINT('Ctrl Pts',(1.93800355965069E-14,6.37500000273118,
105.5));
#10104=CARTESIAN_POINT('Ctrl Pts',(-43.6995308303616,6.31250000273118,105.5));
#10105=CARTESIAN_POINT('Ctrl Pts',(-74.5997654151808,6.25000000273118,74.5997654151808));
#10106=CARTESIAN_POINT('Ctrl Pts',(-105.5,6.18750000273117,43.6995308303616));
#10107=CARTESIAN_POINT('Ctrl Pts',(-105.5,6.12500000273117,0.));
#10108=CARTESIAN_POINT('Ctrl Pts',(-105.5,6.06250000273118,-43.6995308303615));
#10109=CARTESIAN_POINT('Ctrl Pts',(-74.5997654151808,6.00000000273118,-74.5997654151808));
#10110=CARTESIAN_POINT('Ctrl Pts',(-43.6995308303615,5.93750000273118,-105.5));
#10111=CARTESIAN_POINT('Ctrl Pts',(-6.46001186550229E-15,5.87500000273117,
-105.5));
#10112=CARTESIAN_POINT('Ctrl Pts',(43.6995308303615,5.81250000273117,-105.5));
#10113=CARTESIAN_POINT('Ctrl Pts',(74.5997654151808,5.75000000273118,-74.5997654151808));
#10114=CARTESIAN_POINT('Ctrl Pts',(105.5,5.68750000273117,-43.6995308303616));
#10115=CARTESIAN_POINT('Ctrl Pts',(105.5,5.62500000273117,-1.29200237310046E-14));
#10116=CARTESIAN_POINT('Ctrl Pts',(105.5,5.56250000273117,43.6995308303615));
#10117=CARTESIAN_POINT('Ctrl Pts',(74.5997654151808,5.50000000273117,74.5997654151808));
#10118=CARTESIAN_POINT('Ctrl Pts',(43.6995308303616,5.43750000273118,105.5));
#10119=CARTESIAN_POINT('Ctrl Pts',(1.93800355965069E-14,5.37500000273117,
105.5));
#10120=CARTESIAN_POINT('Ctrl Pts',(-43.6995308303616,5.31250000273117,105.5));
#10121=CARTESIAN_POINT('Ctrl Pts',(-74.5997654151808,5.25000000273117,74.5997654151808));
#10122=CARTESIAN_POINT('Ctrl Pts',(-105.5,5.18750000273117,43.6995308303616));
#10123=CARTESIAN_POINT('Ctrl Pts',(-105.5,5.12500000273118,0.));
#10124=CARTESIAN_POINT('Ctrl Pts',(-105.5,5.06250000273118,-43.6995308303615));
#10125=CARTESIAN_POINT('Ctrl Pts',(-74.5997654151808,5.00000000273118,-74.5997654151808));
#10126=CARTESIAN_POINT('Ctrl Pts',(-43.6995308303615,4.93750000273118,-105.5));
#10127=CARTESIAN_POINT('Ctrl Pts',(-6.46001186550229E-15,4.87500000273118,
-105.5));
#10128=CARTESIAN_POINT('Ctrl Pts',(43.6995308303615,4.81250000273118,-105.5));
#10129=CARTESIAN_POINT('Ctrl Pts',(74.5997654151808,4.75000000273118,-74.5997654151808));
#10130=CARTESIAN_POINT('Ctrl Pts',(105.5,4.68750000273118,-43.6995308303616));
#10131=CARTESIAN_POINT('Ctrl Pts',(105.5,4.62500000273118,-1.29200237310046E-14));
#10132=CARTESIAN_POINT('Ctrl Pts',(105.5,4.56250000273118,43.6995308303615));
#10133=CARTESIAN_POINT('Ctrl Pts',(74.5997654151808,4.50000000273118,74.5997654151808));
#10134=CARTESIAN_POINT('Ctrl Pts',(43.6995308303616,4.43750000273118,105.5));
#10135=CARTESIAN_POINT('Ctrl Pts',(1.93800355965069E-14,4.37500000273118,
105.5));
#10136=CARTESIAN_POINT('Ctrl Pts',(-43.6995308303616,4.31250000273118,105.5));
#10137=CARTESIAN_POINT('Ctrl Pts',(-74.5997654151808,4.25000000273118,74.5997654151808));
#10138=CARTESIAN_POINT('Ctrl Pts',(-105.5,4.18750000273118,43.6995308303616));
#10139=CARTESIAN_POINT('Ctrl Pts',(-105.5,4.12500000273118,0.));
#10140=CARTESIAN_POINT('Ctrl Pts',(-105.5,4.06250000273118,-43.6995308303615));
#10141=CARTESIAN_POINT('Ctrl Pts',(-74.5997654151808,4.00000000273118,-74.5997654151808));
#10142=CARTESIAN_POINT('Ctrl Pts',(-43.6995308303615,3.93750000273118,-105.5));
#10143=CARTESIAN_POINT('Ctrl Pts',(-6.46001186550229E-15,3.87500000273118,
-105.5));
#10144=CARTESIAN_POINT('Ctrl Pts',(43.6995308303615,3.81250000273118,-105.5));
#10145=CARTESIAN_POINT('Ctrl Pts',(74.5997654151808,3.75000000273118,-74.5997654151808));
#10146=CARTESIAN_POINT('Ctrl Pts',(105.5,3.68750000273118,-43.6995308303616));
#10147=CARTESIAN_POINT('Ctrl Pts',(105.5,3.62500000273118,-1.29200237310046E-14));
#10148=CARTESIAN_POINT('Ctrl Pts',(105.5,3.56250000273118,43.6995308303615));
#10149=CARTESIAN_POINT('Ctrl Pts',(74.5997654151808,3.50000000273118,74.5997654151808));
#10150=CARTESIAN_POINT('Ctrl Pts',(43.6995308303616,3.43750000273118,105.5));
#10151=CARTESIAN_POINT('Ctrl Pts',(1.93800355965069E-14,3.37500000273118,
105.5));
#10152=CARTESIAN_POINT('Ctrl Pts',(-43.6995308303616,3.31250000273118,105.5));
#10153=CARTESIAN_POINT('Ctrl Pts',(-74.5997654151808,3.25000000273118,74.5997654151808));
#10154=CARTESIAN_POINT('Ctrl Pts',(-105.5,3.18750000273118,43.6995308303616));
#10155=CARTESIAN_POINT('Ctrl Pts',(-105.5,3.12500000273118,0.));
#10156=CARTESIAN_POINT('Ctrl Pts',(-105.5,3.06250000273118,-43.6995308303615));
#10157=CARTESIAN_POINT('Ctrl Pts',(-74.5997654151808,3.00000000273118,-74.5997654151808));
#10158=CARTESIAN_POINT('Ctrl Pts',(-43.6995308303615,2.93750000273118,-105.5));
#10159=CARTESIAN_POINT('Ctrl Pts',(-6.46001186550229E-15,2.87500000273118,
-105.5));
#10160=CARTESIAN_POINT('Ctrl Pts',(43.6995308303615,2.81250000273118,-105.5));
#10161=CARTESIAN_POINT('Ctrl Pts',(74.5997654151808,2.75000000273118,-74.5997654151808));
#10162=CARTESIAN_POINT('Ctrl Pts',(105.5,2.68750000273118,-43.6995308303616));
#10163=CARTESIAN_POINT('Ctrl Pts',(105.5,2.62500000273118,-1.29200237310046E-14));
#10164=CARTESIAN_POINT('Ctrl Pts',(105.5,2.56250000273118,43.6995308303615));
#10165=CARTESIAN_POINT('Ctrl Pts',(74.5997654151808,2.50000000273118,74.5997654151808));
#10166=CARTESIAN_POINT('Ctrl Pts',(43.6995308303616,2.43750000273118,105.5));
#10167=CARTESIAN_POINT('Ctrl Pts',(1.93800355965069E-14,2.37500000273118,
105.5));
#10168=CARTESIAN_POINT('Ctrl Pts',(-43.6995308303616,2.31250000273118,105.5));
#10169=CARTESIAN_POINT('Ctrl Pts',(-74.5997654151808,2.25000000273118,74.5997654151808));
#10170=CARTESIAN_POINT('Ctrl Pts',(-105.5,2.18750000273118,43.6995308303616));
#10171=CARTESIAN_POINT('Ctrl Pts',(-105.5,2.12500000273118,0.));
#10172=CARTESIAN_POINT('Ctrl Pts',(-105.5,2.06250000273118,-43.6995308303615));
#10173=CARTESIAN_POINT('Ctrl Pts',(-74.5997654151808,2.00000000273118,-74.5997654151808));
#10174=CARTESIAN_POINT('Ctrl Pts',(-43.6995308303615,1.93750000273118,-105.5));
#10175=CARTESIAN_POINT('Ctrl Pts',(-6.46001186550229E-15,1.87500000273118,
-105.5));
#10176=CARTESIAN_POINT('Ctrl Pts',(43.6995308303615,1.81250000273118,-105.5));
#10177=CARTESIAN_POINT('Ctrl Pts',(74.5997654151808,1.75000000273118,-74.5997654151808));
#10178=CARTESIAN_POINT('Ctrl Pts',(105.5,1.68750000273118,-43.6995308303616));
#10179=CARTESIAN_POINT('Ctrl Pts',(105.5,1.62500000273118,-1.29200237310046E-14));
#10180=CARTESIAN_POINT('Ctrl Pts',(105.5,1.56250000273118,43.6995308303615));
#10181=CARTESIAN_POINT('Ctrl Pts',(74.5997654151808,1.50000000273118,74.5997654151808));
#10182=CARTESIAN_POINT('Ctrl Pts',(43.6995308303616,1.43750000273118,105.5));
#10183=CARTESIAN_POINT('Ctrl Pts',(1.93800355965069E-14,1.37500000273118,
105.5));
#10184=CARTESIAN_POINT('Ctrl Pts',(-43.6995308303616,1.31250000273118,105.5));
#10185=CARTESIAN_POINT('Ctrl Pts',(-74.5997654151808,1.25000000273118,74.5997654151808));
#10186=CARTESIAN_POINT('Ctrl Pts',(-105.5,1.18750000273118,43.6995308303616));
#10187=CARTESIAN_POINT('Ctrl Pts',(-105.5,1.12500000273118,0.));
#10188=CARTESIAN_POINT('Ctrl Pts',(-105.5,1.06250000273118,-43.6995308303615));
#10189=CARTESIAN_POINT('Ctrl Pts',(-74.5997654151808,1.00000000273118,-74.5997654151808));
#10190=CARTESIAN_POINT('Ctrl Pts',(-43.6995308303615,0.937500002731177,
-105.5));
#10191=CARTESIAN_POINT('Ctrl Pts',(-6.46001186550229E-15,0.875000002731177,
-105.5));
#10192=CARTESIAN_POINT('Ctrl Pts',(43.6995308303615,0.812500002731177,-105.5));
#10193=CARTESIAN_POINT('Ctrl Pts',(74.5997654151808,0.750000002731177,-74.5997654151808));
#10194=CARTESIAN_POINT('Ctrl Pts',(105.5,0.687500002731177,-43.6995308303616));
#10195=CARTESIAN_POINT('Ctrl Pts',(105.5,0.625000002731177,-1.29200237310046E-14));
#10196=CARTESIAN_POINT('Ctrl Pts',(105.5,0.562500002731177,43.6995308303615));
#10197=CARTESIAN_POINT('Ctrl Pts',(74.5997654151808,0.500000002731177,74.5997654151808));
#10198=CARTESIAN_POINT('Ctrl Pts',(43.6995308303616,0.437500002731177,105.5));
#10199=CARTESIAN_POINT('Ctrl Pts',(1.93800355965069E-14,0.375000002731177,
105.5));
#10200=CARTESIAN_POINT('Ctrl Pts',(-43.6995308303616,0.312500002731177,
105.5));
#10201=CARTESIAN_POINT('Ctrl Pts',(-74.5997654151808,0.250000002731177,
74.5997654151808));
#10202=CARTESIAN_POINT('Ctrl Pts',(-105.5,0.187500002731177,43.6995308303616));
#10203=CARTESIAN_POINT('Ctrl Pts',(-105.5,0.125000002731177,0.));
#10204=CARTESIAN_POINT('Ctrl Pts',(-105.5,0.0625000027311765,-43.6995308303615));
#10205=CARTESIAN_POINT('Ctrl Pts',(-74.5997654151808,2.7311763961535E-9,
-74.5997654151808));
#10206=CARTESIAN_POINT('Ctrl Pts',(-43.6995308303615,-0.0624999972688237,
-105.5));
#10207=CARTESIAN_POINT('Ctrl Pts',(-6.46001186550229E-15,-0.124999997268824,
-105.5));
#10208=CARTESIAN_POINT('Ctrl Pts',(43.6995308303615,-0.187499997268824,
-105.5));
#10209=CARTESIAN_POINT('Ctrl Pts',(74.5997654151808,-0.249999997268824,
-74.5997654151808));
#10210=CARTESIAN_POINT('Ctrl Pts',(105.5,-0.312499997268824,-43.6995308303616));
#10211=CARTESIAN_POINT('Ctrl Pts',(105.5,-0.374999997268824,-1.29200237310046E-14));
#10212=CARTESIAN_POINT('Ctrl Pts',(105.5,-0.437499997268824,43.6995308303615));
#10213=CARTESIAN_POINT('Ctrl Pts',(74.5997654151808,-0.499999997268824,
74.5997654151808));
#10214=CARTESIAN_POINT('Ctrl Pts',(43.6995308303616,-0.562499997268824,
105.5));
#10215=CARTESIAN_POINT('Ctrl Pts',(1.93800355965069E-14,-0.624999997268824,
105.5));
#10216=CARTESIAN_POINT('Ctrl Pts',(-43.6995308303616,-0.687499997268824,
105.5));
#10217=CARTESIAN_POINT('Ctrl Pts',(-74.5997654151808,-0.749999997268824,
74.5997654151808));
#10218=CARTESIAN_POINT('Ctrl Pts',(-105.5,-0.812499997268824,43.6995308303616));
#10219=CARTESIAN_POINT('Ctrl Pts',(-105.5,-0.874999997268824,0.));
#10220=CARTESIAN_POINT('Ctrl Pts',(-104.958734125,49.4375000013656,0.));
#10221=CARTESIAN_POINT('Ctrl Pts',(-104.958734125,49.3750000013656,-43.4753311640868));
#10222=CARTESIAN_POINT('Ctrl Pts',(-74.2170326445434,49.3125000013656,-74.2170326445434));
#10223=CARTESIAN_POINT('Ctrl Pts',(-43.4753311640868,49.2500000013656,-104.958734125));
#10224=CARTESIAN_POINT('Ctrl Pts',(-6.42686888943697E-15,49.1875000013656,
-104.958734125));
#10225=CARTESIAN_POINT('Ctrl Pts',(43.4753311640868,49.1250000013656,-104.958734125));
#10226=CARTESIAN_POINT('Ctrl Pts',(74.2170326445434,49.0625000013656,-74.2170326445434));
#10227=CARTESIAN_POINT('Ctrl Pts',(104.958734125,49.0000000013656,-43.4753311640868));
#10228=CARTESIAN_POINT('Ctrl Pts',(104.958734125,48.9375000013656,-1.28537377788739E-14));
#10229=CARTESIAN_POINT('Ctrl Pts',(104.958734125,48.8750000013656,43.4753311640868));
#10230=CARTESIAN_POINT('Ctrl Pts',(74.2170326445434,48.8125000013656,74.2170326445434));
#10231=CARTESIAN_POINT('Ctrl Pts',(43.4753311640869,48.7500000013656,104.958734125));
#10232=CARTESIAN_POINT('Ctrl Pts',(1.92806066683109E-14,48.6875000013656,
104.958734125));
#10233=CARTESIAN_POINT('Ctrl Pts',(-43.4753311640868,48.6250000013656,104.958734125));
#10234=CARTESIAN_POINT('Ctrl Pts',(-74.2170326445434,48.5625000013656,74.2170326445434));
#10235=CARTESIAN_POINT('Ctrl Pts',(-104.958734125,48.5000000013656,43.4753311640869));
#10236=CARTESIAN_POINT('Ctrl Pts',(-104.958734125,48.4375000013656,0.));
#10237=CARTESIAN_POINT('Ctrl Pts',(-104.958734125,48.3750000013656,-43.4753311640868));
#10238=CARTESIAN_POINT('Ctrl Pts',(-74.2170326445434,48.3125000013656,-74.2170326445434));
#10239=CARTESIAN_POINT('Ctrl Pts',(-43.4753311640868,48.2500000013656,-104.958734125));
#10240=CARTESIAN_POINT('Ctrl Pts',(-6.42686888943697E-15,48.1875000013656,
-104.958734125));
#10241=CARTESIAN_POINT('Ctrl Pts',(43.4753311640868,48.1250000013656,-104.958734125));
#10242=CARTESIAN_POINT('Ctrl Pts',(74.2170326445434,48.0625000013656,-74.2170326445434));
#10243=CARTESIAN_POINT('Ctrl Pts',(104.958734125,48.0000000013656,-43.4753311640868));
#10244=CARTESIAN_POINT('Ctrl Pts',(104.958734125,47.9375000013656,-1.28537377788739E-14));
#10245=CARTESIAN_POINT('Ctrl Pts',(104.958734125,47.8750000013656,43.4753311640868));
#10246=CARTESIAN_POINT('Ctrl Pts',(74.2170326445434,47.8125000013656,74.2170326445434));
#10247=CARTESIAN_POINT('Ctrl Pts',(43.4753311640869,47.7500000013656,104.958734125));
#10248=CARTESIAN_POINT('Ctrl Pts',(1.92806066683109E-14,47.6875000013656,
104.958734125));
#10249=CARTESIAN_POINT('Ctrl Pts',(-43.4753311640868,47.6250000013656,104.958734125));
#10250=CARTESIAN_POINT('Ctrl Pts',(-74.2170326445434,47.5625000013656,74.2170326445434));
#10251=CARTESIAN_POINT('Ctrl Pts',(-104.958734125,47.5000000013656,43.4753311640869));
#10252=CARTESIAN_POINT('Ctrl Pts',(-104.958734125,47.4375000013656,0.));
#10253=CARTESIAN_POINT('Ctrl Pts',(-104.958734125,47.3750000013656,-43.4753311640868));
#10254=CARTESIAN_POINT('Ctrl Pts',(-74.2170326445434,47.3125000013656,-74.2170326445434));
#10255=CARTESIAN_POINT('Ctrl Pts',(-43.4753311640868,47.2500000013656,-104.958734125));
#10256=CARTESIAN_POINT('Ctrl Pts',(-6.42686888943697E-15,47.1875000013656,
-104.958734125));
#10257=CARTESIAN_POINT('Ctrl Pts',(43.4753311640868,47.1250000013656,-104.958734125));
#10258=CARTESIAN_POINT('Ctrl Pts',(74.2170326445434,47.0625000013656,-74.2170326445434));
#10259=CARTESIAN_POINT('Ctrl Pts',(104.958734125,47.0000000013656,-43.4753311640868));
#10260=CARTESIAN_POINT('Ctrl Pts',(104.958734125,46.9375000013656,-1.28537377788739E-14));
#10261=CARTESIAN_POINT('Ctrl Pts',(104.958734125,46.8750000013656,43.4753311640868));
#10262=CARTESIAN_POINT('Ctrl Pts',(74.2170326445434,46.8125000013656,74.2170326445434));
#10263=CARTESIAN_POINT('Ctrl Pts',(43.4753311640869,46.7500000013656,104.958734125));
#10264=CARTESIAN_POINT('Ctrl Pts',(1.92806066683109E-14,46.6875000013656,
104.958734125));
#10265=CARTESIAN_POINT('Ctrl Pts',(-43.4753311640868,46.6250000013656,104.958734125));
#10266=CARTESIAN_POINT('Ctrl Pts',(-74.2170326445434,46.5625000013656,74.2170326445434));
#10267=CARTESIAN_POINT('Ctrl Pts',(-104.958734125,46.5000000013656,43.4753311640869));
#10268=CARTESIAN_POINT('Ctrl Pts',(-104.958734125,46.4375000013656,0.));
#10269=CARTESIAN_POINT('Ctrl Pts',(-104.958734125,46.3750000013656,-43.4753311640868));
#10270=CARTESIAN_POINT('Ctrl Pts',(-74.2170326445434,46.3125000013656,-74.2170326445434));
#10271=CARTESIAN_POINT('Ctrl Pts',(-43.4753311640868,46.2500000013656,-104.958734125));
#10272=CARTESIAN_POINT('Ctrl Pts',(-6.42686888943697E-15,46.1875000013656,
-104.958734125));
#10273=CARTESIAN_POINT('Ctrl Pts',(43.4753311640868,46.1250000013656,-104.958734125));
#10274=CARTESIAN_POINT('Ctrl Pts',(74.2170326445434,46.0625000013656,-74.2170326445434));
#10275=CARTESIAN_POINT('Ctrl Pts',(104.958734125,46.0000000013656,-43.4753311640868));
#10276=CARTESIAN_POINT('Ctrl Pts',(104.958734125,45.9375000013656,-1.28537377788739E-14));
#10277=CARTESIAN_POINT('Ctrl Pts',(104.958734125,45.8750000013656,43.4753311640868));
#10278=CARTESIAN_POINT('Ctrl Pts',(74.2170326445434,45.8125000013656,74.2170326445434));
#10279=CARTESIAN_POINT('Ctrl Pts',(43.4753311640869,45.7500000013656,104.958734125));
#10280=CARTESIAN_POINT('Ctrl Pts',(1.92806066683109E-14,45.6875000013656,
104.958734125));
#10281=CARTESIAN_POINT('Ctrl Pts',(-43.4753311640868,45.6250000013656,104.958734125));
#10282=CARTESIAN_POINT('Ctrl Pts',(-74.2170326445434,45.5625000013656,74.2170326445434));
#10283=CARTESIAN_POINT('Ctrl Pts',(-104.958734125,45.5000000013656,43.4753311640869));
#10284=CARTESIAN_POINT('Ctrl Pts',(-104.958734125,45.4375000013656,0.));
#10285=CARTESIAN_POINT('Ctrl Pts',(-104.958734125,45.3750000013656,-43.4753311640868));
#10286=CARTESIAN_POINT('Ctrl Pts',(-74.2170326445434,45.3125000013656,-74.2170326445434));
#10287=CARTESIAN_POINT('Ctrl Pts',(-43.4753311640868,45.2500000013656,-104.958734125));
#10288=CARTESIAN_POINT('Ctrl Pts',(-6.42686888943697E-15,45.1875000013656,
-104.958734125));
#10289=CARTESIAN_POINT('Ctrl Pts',(43.4753311640868,45.1250000013656,-104.958734125));
#10290=CARTESIAN_POINT('Ctrl Pts',(74.2170326445434,45.0625000013656,-74.2170326445434));
#10291=CARTESIAN_POINT('Ctrl Pts',(104.958734125,45.0000000013656,-43.4753311640868));
#10292=CARTESIAN_POINT('Ctrl Pts',(104.958734125,44.9375000013656,-1.28537377788739E-14));
#10293=CARTESIAN_POINT('Ctrl Pts',(104.958734125,44.8750000013656,43.4753311640868));
#10294=CARTESIAN_POINT('Ctrl Pts',(74.2170326445434,44.8125000013656,74.2170326445434));
#10295=CARTESIAN_POINT('Ctrl Pts',(43.4753311640869,44.7500000013656,104.958734125));
#10296=CARTESIAN_POINT('Ctrl Pts',(1.92806066683109E-14,44.6875000013656,
104.958734125));
#10297=CARTESIAN_POINT('Ctrl Pts',(-43.4753311640868,44.6250000013656,104.958734125));
#10298=CARTESIAN_POINT('Ctrl Pts',(-74.2170326445434,44.5625000013656,74.2170326445434));
#10299=CARTESIAN_POINT('Ctrl Pts',(-104.958734125,44.5000000013656,43.4753311640869));
#10300=CARTESIAN_POINT('Ctrl Pts',(-104.958734125,44.4375000013656,0.));
#10301=CARTESIAN_POINT('Ctrl Pts',(-104.958734125,44.3750000013656,-43.4753311640868));
#10302=CARTESIAN_POINT('Ctrl Pts',(-74.2170326445434,44.3125000013656,-74.2170326445434));
#10303=CARTESIAN_POINT('Ctrl Pts',(-43.4753311640868,44.2500000013656,-104.958734125));
#10304=CARTESIAN_POINT('Ctrl Pts',(-6.42686888943697E-15,44.1875000013656,
-104.958734125));
#10305=CARTESIAN_POINT('Ctrl Pts',(43.4753311640868,44.1250000013656,-104.958734125));
#10306=CARTESIAN_POINT('Ctrl Pts',(74.2170326445434,44.0625000013656,-74.2170326445434));
#10307=CARTESIAN_POINT('Ctrl Pts',(104.958734125,44.0000000013656,-43.4753311640868));
#10308=CARTESIAN_POINT('Ctrl Pts',(104.958734125,43.9375000013656,-1.28537377788739E-14));
#10309=CARTESIAN_POINT('Ctrl Pts',(104.958734125,43.8750000013656,43.4753311640868));
#10310=CARTESIAN_POINT('Ctrl Pts',(74.2170326445434,43.8125000013656,74.2170326445434));
#10311=CARTESIAN_POINT('Ctrl Pts',(43.4753311640869,43.7500000013656,104.958734125));
#10312=CARTESIAN_POINT('Ctrl Pts',(1.92806066683109E-14,43.6875000013656,
104.958734125));
#10313=CARTESIAN_POINT('Ctrl Pts',(-43.4753311640868,43.6250000013656,104.958734125));
#10314=CARTESIAN_POINT('Ctrl Pts',(-74.2170326445434,43.5625000013656,74.2170326445434));
#10315=CARTESIAN_POINT('Ctrl Pts',(-104.958734125,43.5000000013656,43.4753311640869));
#10316=CARTESIAN_POINT('Ctrl Pts',(-104.958734125,43.4375000013656,0.));
#10317=CARTESIAN_POINT('Ctrl Pts',(-104.958734125,43.3750000013656,-43.4753311640868));
#10318=CARTESIAN_POINT('Ctrl Pts',(-74.2170326445434,43.3125000013656,-74.2170326445434));
#10319=CARTESIAN_POINT('Ctrl Pts',(-43.4753311640868,43.2500000013656,-104.958734125));
#10320=CARTESIAN_POINT('Ctrl Pts',(-6.42686888943697E-15,43.1875000013656,
-104.958734125));
#10321=CARTESIAN_POINT('Ctrl Pts',(43.4753311640868,43.1250000013656,-104.958734125));
#10322=CARTESIAN_POINT('Ctrl Pts',(74.2170326445434,43.0625000013656,-74.2170326445434));
#10323=CARTESIAN_POINT('Ctrl Pts',(104.958734125,43.0000000013656,-43.4753311640868));
#10324=CARTESIAN_POINT('Ctrl Pts',(104.958734125,42.9375000013656,-1.28537377788739E-14));
#10325=CARTESIAN_POINT('Ctrl Pts',(104.958734125,42.8750000013656,43.4753311640868));
#10326=CARTESIAN_POINT('Ctrl Pts',(74.2170326445434,42.8125000013656,74.2170326445434));
#10327=CARTESIAN_POINT('Ctrl Pts',(43.4753311640869,42.7500000013656,104.958734125));
#10328=CARTESIAN_POINT('Ctrl Pts',(1.92806066683109E-14,42.6875000013656,
104.958734125));
#10329=CARTESIAN_POINT('Ctrl Pts',(-43.4753311640868,42.6250000013656,104.958734125));
#10330=CARTESIAN_POINT('Ctrl Pts',(-74.2170326445434,42.5625000013656,74.2170326445434));
#10331=CARTESIAN_POINT('Ctrl Pts',(-104.958734125,42.5000000013656,43.4753311640869));
#10332=CARTESIAN_POINT('Ctrl Pts',(-104.958734125,42.4375000013656,0.));
#10333=CARTESIAN_POINT('Ctrl Pts',(-104.958734125,42.3750000013656,-43.4753311640868));
#10334=CARTESIAN_POINT('Ctrl Pts',(-74.2170326445434,42.3125000013656,-74.2170326445434));
#10335=CARTESIAN_POINT('Ctrl Pts',(-43.4753311640868,42.2500000013656,-104.958734125));
#10336=CARTESIAN_POINT('Ctrl Pts',(-6.42686888943697E-15,42.1875000013656,
-104.958734125));
#10337=CARTESIAN_POINT('Ctrl Pts',(43.4753311640868,42.1250000013656,-104.958734125));
#10338=CARTESIAN_POINT('Ctrl Pts',(74.2170326445434,42.0625000013656,-74.2170326445434));
#10339=CARTESIAN_POINT('Ctrl Pts',(104.958734125,42.0000000013656,-43.4753311640868));
#10340=CARTESIAN_POINT('Ctrl Pts',(104.958734125,41.9375000013656,-1.28537377788739E-14));
#10341=CARTESIAN_POINT('Ctrl Pts',(104.958734125,41.8750000013656,43.4753311640868));
#10342=CARTESIAN_POINT('Ctrl Pts',(74.2170326445434,41.8125000013656,74.2170326445434));
#10343=CARTESIAN_POINT('Ctrl Pts',(43.4753311640869,41.7500000013656,104.958734125));
#10344=CARTESIAN_POINT('Ctrl Pts',(1.92806066683109E-14,41.6875000013656,
104.958734125));
#10345=CARTESIAN_POINT('Ctrl Pts',(-43.4753311640868,41.6250000013656,104.958734125));
#10346=CARTESIAN_POINT('Ctrl Pts',(-74.2170326445434,41.5625000013656,74.2170326445434));
#10347=CARTESIAN_POINT('Ctrl Pts',(-104.958734125,41.5000000013656,43.4753311640869));
#10348=CARTESIAN_POINT('Ctrl Pts',(-104.958734125,41.4375000013656,0.));
#10349=CARTESIAN_POINT('Ctrl Pts',(-104.958734125,41.3750000013656,-43.4753311640868));
#10350=CARTESIAN_POINT('Ctrl Pts',(-74.2170326445434,41.3125000013656,-74.2170326445434));
#10351=CARTESIAN_POINT('Ctrl Pts',(-43.4753311640868,41.2500000013656,-104.958734125));
#10352=CARTESIAN_POINT('Ctrl Pts',(-6.42686888943697E-15,41.1875000013656,
-104.958734125));
#10353=CARTESIAN_POINT('Ctrl Pts',(43.4753311640868,41.1250000013656,-104.958734125));
#10354=CARTESIAN_POINT('Ctrl Pts',(74.2170326445434,41.0625000013656,-74.2170326445434));
#10355=CARTESIAN_POINT('Ctrl Pts',(104.958734125,41.0000000013656,-43.4753311640868));
#10356=CARTESIAN_POINT('Ctrl Pts',(104.958734125,40.9375000013656,-1.28537377788739E-14));
#10357=CARTESIAN_POINT('Ctrl Pts',(104.958734125,40.8750000013656,43.4753311640868));
#10358=CARTESIAN_POINT('Ctrl Pts',(74.2170326445434,40.8125000013656,74.2170326445434));
#10359=CARTESIAN_POINT('Ctrl Pts',(43.4753311640869,40.7500000013656,104.958734125));
#10360=CARTESIAN_POINT('Ctrl Pts',(1.92806066683109E-14,40.6875000013656,
104.958734125));
#10361=CARTESIAN_POINT('Ctrl Pts',(-43.4753311640868,40.6250000013656,104.958734125));
#10362=CARTESIAN_POINT('Ctrl Pts',(-74.2170326445434,40.5625000013656,74.2170326445434));
#10363=CARTESIAN_POINT('Ctrl Pts',(-104.958734125,40.5000000013656,43.4753311640869));
#10364=CARTESIAN_POINT('Ctrl Pts',(-104.958734125,40.4375000013656,0.));
#10365=CARTESIAN_POINT('Ctrl Pts',(-104.958734125,40.3750000013656,-43.4753311640868));
#10366=CARTESIAN_POINT('Ctrl Pts',(-74.2170326445434,40.3125000013656,-74.2170326445434));
#10367=CARTESIAN_POINT('Ctrl Pts',(-43.4753311640868,40.2500000013656,-104.958734125));
#10368=CARTESIAN_POINT('Ctrl Pts',(-6.42686888943697E-15,40.1875000013656,
-104.958734125));
#10369=CARTESIAN_POINT('Ctrl Pts',(43.4753311640868,40.1250000013656,-104.958734125));
#10370=CARTESIAN_POINT('Ctrl Pts',(74.2170326445434,40.0625000013656,-74.2170326445434));
#10371=CARTESIAN_POINT('Ctrl Pts',(104.958734125,40.0000000013656,-43.4753311640868));
#10372=CARTESIAN_POINT('Ctrl Pts',(104.958734125,39.9375000013656,-1.28537377788739E-14));
#10373=CARTESIAN_POINT('Ctrl Pts',(104.958734125,39.8750000013656,43.4753311640868));
#10374=CARTESIAN_POINT('Ctrl Pts',(74.2170326445434,39.8125000013656,74.2170326445434));
#10375=CARTESIAN_POINT('Ctrl Pts',(43.4753311640869,39.7500000013656,104.958734125));
#10376=CARTESIAN_POINT('Ctrl Pts',(1.92806066683109E-14,39.6875000013656,
104.958734125));
#10377=CARTESIAN_POINT('Ctrl Pts',(-43.4753311640868,39.6250000013656,104.958734125));
#10378=CARTESIAN_POINT('Ctrl Pts',(-74.2170326445434,39.5625000013656,74.2170326445434));
#10379=CARTESIAN_POINT('Ctrl Pts',(-104.958734125,39.5000000013656,43.4753311640869));
#10380=CARTESIAN_POINT('Ctrl Pts',(-104.958734125,39.4375000013656,0.));
#10381=CARTESIAN_POINT('Ctrl Pts',(-104.958734125,39.3750000013656,-43.4753311640868));
#10382=CARTESIAN_POINT('Ctrl Pts',(-74.2170326445434,39.3125000013656,-74.2170326445434));
#10383=CARTESIAN_POINT('Ctrl Pts',(-43.4753311640868,39.2500000013656,-104.958734125));
#10384=CARTESIAN_POINT('Ctrl Pts',(-6.42686888943697E-15,39.1875000013656,
-104.958734125));
#10385=CARTESIAN_POINT('Ctrl Pts',(43.4753311640868,39.1250000013656,-104.958734125));
#10386=CARTESIAN_POINT('Ctrl Pts',(74.2170326445434,39.0625000013656,-74.2170326445434));
#10387=CARTESIAN_POINT('Ctrl Pts',(104.958734125,39.0000000013656,-43.4753311640868));
#10388=CARTESIAN_POINT('Ctrl Pts',(104.958734125,38.9375000013656,-1.28537377788739E-14));
#10389=CARTESIAN_POINT('Ctrl Pts',(104.958734125,38.8750000013656,43.4753311640868));
#10390=CARTESIAN_POINT('Ctrl Pts',(74.2170326445434,38.8125000013656,74.2170326445434));
#10391=CARTESIAN_POINT('Ctrl Pts',(43.4753311640869,38.7500000013656,104.958734125));
#10392=CARTESIAN_POINT('Ctrl Pts',(1.92806066683109E-14,38.6875000013656,
104.958734125));
#10393=CARTESIAN_POINT('Ctrl Pts',(-43.4753311640868,38.6250000013656,104.958734125));
#10394=CARTESIAN_POINT('Ctrl Pts',(-74.2170326445434,38.5625000013656,74.2170326445434));
#10395=CARTESIAN_POINT('Ctrl Pts',(-104.958734125,38.5000000013656,43.4753311640869));
#10396=CARTESIAN_POINT('Ctrl Pts',(-104.958734125,38.4375000013656,0.));
#10397=CARTESIAN_POINT('Ctrl Pts',(-104.958734125,38.3750000013656,-43.4753311640868));
#10398=CARTESIAN_POINT('Ctrl Pts',(-74.2170326445434,38.3125000013656,-74.2170326445434));
#10399=CARTESIAN_POINT('Ctrl Pts',(-43.4753311640868,38.2500000013656,-104.958734125));
#10400=CARTESIAN_POINT('Ctrl Pts',(-6.42686888943697E-15,38.1875000013656,
-104.958734125));
#10401=CARTESIAN_POINT('Ctrl Pts',(43.4753311640868,38.1250000013656,-104.958734125));
#10402=CARTESIAN_POINT('Ctrl Pts',(74.2170326445434,38.0625000013656,-74.2170326445434));
#10403=CARTESIAN_POINT('Ctrl Pts',(104.958734125,38.0000000013656,-43.4753311640868));
#10404=CARTESIAN_POINT('Ctrl Pts',(104.958734125,37.9375000013656,-1.28537377788739E-14));
#10405=CARTESIAN_POINT('Ctrl Pts',(104.958734125,37.8750000013656,43.4753311640868));
#10406=CARTESIAN_POINT('Ctrl Pts',(74.2170326445434,37.8125000013656,74.2170326445434));
#10407=CARTESIAN_POINT('Ctrl Pts',(43.4753311640869,37.7500000013656,104.958734125));
#10408=CARTESIAN_POINT('Ctrl Pts',(1.92806066683109E-14,37.6875000013656,
104.958734125));
#10409=CARTESIAN_POINT('Ctrl Pts',(-43.4753311640868,37.6250000013656,104.958734125));
#10410=CARTESIAN_POINT('Ctrl Pts',(-74.2170326445434,37.5625000013656,74.2170326445434));
#10411=CARTESIAN_POINT('Ctrl Pts',(-104.958734125,37.5000000013656,43.4753311640869));
#10412=CARTESIAN_POINT('Ctrl Pts',(-104.958734125,37.4375000013656,0.));
#10413=CARTESIAN_POINT('Ctrl Pts',(-104.958734125,37.3750000013656,-43.4753311640868));
#10414=CARTESIAN_POINT('Ctrl Pts',(-74.2170326445434,37.3125000013656,-74.2170326445434));
#10415=CARTESIAN_POINT('Ctrl Pts',(-43.4753311640868,37.2500000013656,-104.958734125));
#10416=CARTESIAN_POINT('Ctrl Pts',(-6.42686888943697E-15,37.1875000013656,
-104.958734125));
#10417=CARTESIAN_POINT('Ctrl Pts',(43.4753311640868,37.1250000013656,-104.958734125));
#10418=CARTESIAN_POINT('Ctrl Pts',(74.2170326445434,37.0625000013656,-74.2170326445434));
#10419=CARTESIAN_POINT('Ctrl Pts',(104.958734125,37.0000000013656,-43.4753311640868));
#10420=CARTESIAN_POINT('Ctrl Pts',(104.958734125,36.9375000013656,-1.28537377788739E-14));
#10421=CARTESIAN_POINT('Ctrl Pts',(104.958734125,36.8750000013656,43.4753311640868));
#10422=CARTESIAN_POINT('Ctrl Pts',(74.2170326445434,36.8125000013656,74.2170326445434));
#10423=CARTESIAN_POINT('Ctrl Pts',(43.4753311640869,36.7500000013656,104.958734125));
#10424=CARTESIAN_POINT('Ctrl Pts',(1.92806066683109E-14,36.6875000013656,
104.958734125));
#10425=CARTESIAN_POINT('Ctrl Pts',(-43.4753311640868,36.6250000013656,104.958734125));
#10426=CARTESIAN_POINT('Ctrl Pts',(-74.2170326445434,36.5625000013656,74.2170326445434));
#10427=CARTESIAN_POINT('Ctrl Pts',(-104.958734125,36.5000000013656,43.4753311640869));
#10428=CARTESIAN_POINT('Ctrl Pts',(-104.958734125,36.4375000013656,0.));
#10429=CARTESIAN_POINT('Ctrl Pts',(-104.958734125,36.3750000013656,-43.4753311640868));
#10430=CARTESIAN_POINT('Ctrl Pts',(-74.2170326445434,36.3125000013656,-74.2170326445434));
#10431=CARTESIAN_POINT('Ctrl Pts',(-43.4753311640868,36.2500000013656,-104.958734125));
#10432=CARTESIAN_POINT('Ctrl Pts',(-6.42686888943697E-15,36.1875000013656,
-104.958734125));
#10433=CARTESIAN_POINT('Ctrl Pts',(43.4753311640868,36.1250000013656,-104.958734125));
#10434=CARTESIAN_POINT('Ctrl Pts',(74.2170326445434,36.0625000013656,-74.2170326445434));
#10435=CARTESIAN_POINT('Ctrl Pts',(104.958734125,36.0000000013656,-43.4753311640868));
#10436=CARTESIAN_POINT('Ctrl Pts',(104.958734125,35.9375000013656,-1.28537377788739E-14));
#10437=CARTESIAN_POINT('Ctrl Pts',(104.958734125,35.8750000013656,43.4753311640868));
#10438=CARTESIAN_POINT('Ctrl Pts',(74.2170326445434,35.8125000013656,74.2170326445434));
#10439=CARTESIAN_POINT('Ctrl Pts',(43.4753311640869,35.7500000013656,104.958734125));
#10440=CARTESIAN_POINT('Ctrl Pts',(1.92806066683109E-14,35.6875000013656,
104.958734125));
#10441=CARTESIAN_POINT('Ctrl Pts',(-43.4753311640868,35.6250000013656,104.958734125));
#10442=CARTESIAN_POINT('Ctrl Pts',(-74.2170326445434,35.5625000013656,74.2170326445434));
#10443=CARTESIAN_POINT('Ctrl Pts',(-104.958734125,35.5000000013656,43.4753311640869));
#10444=CARTESIAN_POINT('Ctrl Pts',(-104.958734125,35.4375000013656,0.));
#10445=CARTESIAN_POINT('Ctrl Pts',(-104.958734125,35.3750000013656,-43.4753311640868));
#10446=CARTESIAN_POINT('Ctrl Pts',(-74.2170326445434,35.3125000013656,-74.2170326445434));
#10447=CARTESIAN_POINT('Ctrl Pts',(-43.4753311640868,35.2500000013656,-104.958734125));
#10448=CARTESIAN_POINT('Ctrl Pts',(-6.42686888943697E-15,35.1875000013656,
-104.958734125));
#10449=CARTESIAN_POINT('Ctrl Pts',(43.4753311640868,35.1250000013656,-104.958734125));
#10450=CARTESIAN_POINT('Ctrl Pts',(74.2170326445434,35.0625000013656,-74.2170326445434));
#10451=CARTESIAN_POINT('Ctrl Pts',(104.958734125,35.0000000013656,-43.4753311640868));
#10452=CARTESIAN_POINT('Ctrl Pts',(104.958734125,34.9375000013656,-1.28537377788739E-14));
#10453=CARTESIAN_POINT('Ctrl Pts',(104.958734125,34.8750000013656,43.4753311640868));
#10454=CARTESIAN_POINT('Ctrl Pts',(74.2170326445434,34.8125000013656,74.2170326445434));
#10455=CARTESIAN_POINT('Ctrl Pts',(43.4753311640869,34.7500000013656,104.958734125));
#10456=CARTESIAN_POINT('Ctrl Pts',(1.92806066683109E-14,34.6875000013656,
104.958734125));
#10457=CARTESIAN_POINT('Ctrl Pts',(-43.4753311640868,34.6250000013656,104.958734125));
#10458=CARTESIAN_POINT('Ctrl Pts',(-74.2170326445434,34.5625000013656,74.2170326445434));
#10459=CARTESIAN_POINT('Ctrl Pts',(-104.958734125,34.5000000013656,43.4753311640869));
#10460=CARTESIAN_POINT('Ctrl Pts',(-104.958734125,34.4375000013656,0.));
#10461=CARTESIAN_POINT('Ctrl Pts',(-104.958734125,34.3750000013656,-43.4753311640868));
#10462=CARTESIAN_POINT('Ctrl Pts',(-74.2170326445434,34.3125000013656,-74.2170326445434));
#10463=CARTESIAN_POINT('Ctrl Pts',(-43.4753311640868,34.2500000013656,-104.958734125));
#10464=CARTESIAN_POINT('Ctrl Pts',(-6.42686888943697E-15,34.1875000013656,
-104.958734125));
#10465=CARTESIAN_POINT('Ctrl Pts',(43.4753311640868,34.1250000013656,-104.958734125));
#10466=CARTESIAN_POINT('Ctrl Pts',(74.2170326445434,34.0625000013656,-74.2170326445434));
#10467=CARTESIAN_POINT('Ctrl Pts',(104.958734125,34.0000000013656,-43.4753311640868));
#10468=CARTESIAN_POINT('Ctrl Pts',(104.958734125,33.9375000013656,-1.28537377788739E-14));
#10469=CARTESIAN_POINT('Ctrl Pts',(104.958734125,33.8750000013656,43.4753311640868));
#10470=CARTESIAN_POINT('Ctrl Pts',(74.2170326445434,33.8125000013656,74.2170326445434));
#10471=CARTESIAN_POINT('Ctrl Pts',(43.4753311640869,33.7500000013656,104.958734125));
#10472=CARTESIAN_POINT('Ctrl Pts',(1.92806066683109E-14,33.6875000013656,
104.958734125));
#10473=CARTESIAN_POINT('Ctrl Pts',(-43.4753311640868,33.6250000013656,104.958734125));
#10474=CARTESIAN_POINT('Ctrl Pts',(-74.2170326445434,33.5625000013656,74.2170326445434));
#10475=CARTESIAN_POINT('Ctrl Pts',(-104.958734125,33.5000000013656,43.4753311640869));
#10476=CARTESIAN_POINT('Ctrl Pts',(-104.958734125,33.4375000013656,0.));
#10477=CARTESIAN_POINT('Ctrl Pts',(-104.958734125,33.3750000013656,-43.4753311640868));
#10478=CARTESIAN_POINT('Ctrl Pts',(-74.2170326445434,33.3125000013656,-74.2170326445434));
#10479=CARTESIAN_POINT('Ctrl Pts',(-43.4753311640868,33.2500000013656,-104.958734125));
#10480=CARTESIAN_POINT('Ctrl Pts',(-6.42686888943697E-15,33.1875000013656,
-104.958734125));
#10481=CARTESIAN_POINT('Ctrl Pts',(43.4753311640868,33.1250000013656,-104.958734125));
#10482=CARTESIAN_POINT('Ctrl Pts',(74.2170326445434,33.0625000013656,-74.2170326445434));
#10483=CARTESIAN_POINT('Ctrl Pts',(104.958734125,33.0000000013656,-43.4753311640868));
#10484=CARTESIAN_POINT('Ctrl Pts',(104.958734125,32.9375000013656,-1.28537377788739E-14));
#10485=CARTESIAN_POINT('Ctrl Pts',(104.958734125,32.8750000013656,43.4753311640868));
#10486=CARTESIAN_POINT('Ctrl Pts',(74.2170326445434,32.8125000013656,74.2170326445434));
#10487=CARTESIAN_POINT('Ctrl Pts',(43.4753311640869,32.7500000013656,104.958734125));
#10488=CARTESIAN_POINT('Ctrl Pts',(1.92806066683109E-14,32.6875000013656,
104.958734125));
#10489=CARTESIAN_POINT('Ctrl Pts',(-43.4753311640868,32.6250000013656,104.958734125));
#10490=CARTESIAN_POINT('Ctrl Pts',(-74.2170326445434,32.5625000013656,74.2170326445434));
#10491=CARTESIAN_POINT('Ctrl Pts',(-104.958734125,32.5000000013656,43.4753311640869));
#10492=CARTESIAN_POINT('Ctrl Pts',(-104.958734125,32.4375000013656,0.));
#10493=CARTESIAN_POINT('Ctrl Pts',(-104.958734125,32.3750000013656,-43.4753311640868));
#10494=CARTESIAN_POINT('Ctrl Pts',(-74.2170326445434,32.3125000013656,-74.2170326445434));
#10495=CARTESIAN_POINT('Ctrl Pts',(-43.4753311640868,32.2500000013656,-104.958734125));
#10496=CARTESIAN_POINT('Ctrl Pts',(-6.42686888943697E-15,32.1875000013656,
-104.958734125));
#10497=CARTESIAN_POINT('Ctrl Pts',(43.4753311640868,32.1250000013656,-104.958734125));
#10498=CARTESIAN_POINT('Ctrl Pts',(74.2170326445434,32.0625000013656,-74.2170326445434));
#10499=CARTESIAN_POINT('Ctrl Pts',(104.958734125,32.0000000013656,-43.4753311640868));
#10500=CARTESIAN_POINT('Ctrl Pts',(104.958734125,31.9375000013656,-1.28537377788739E-14));
#10501=CARTESIAN_POINT('Ctrl Pts',(104.958734125,31.8750000013656,43.4753311640868));
#10502=CARTESIAN_POINT('Ctrl Pts',(74.2170326445434,31.8125000013656,74.2170326445434));
#10503=CARTESIAN_POINT('Ctrl Pts',(43.4753311640869,31.7500000013656,104.958734125));
#10504=CARTESIAN_POINT('Ctrl Pts',(1.92806066683109E-14,31.6875000013656,
104.958734125));
#10505=CARTESIAN_POINT('Ctrl Pts',(-43.4753311640868,31.6250000013656,104.958734125));
#10506=CARTESIAN_POINT('Ctrl Pts',(-74.2170326445434,31.5625000013656,74.2170326445434));
#10507=CARTESIAN_POINT('Ctrl Pts',(-104.958734125,31.5000000013656,43.4753311640869));
#10508=CARTESIAN_POINT('Ctrl Pts',(-104.958734125,31.4375000013656,0.));
#10509=CARTESIAN_POINT('Ctrl Pts',(-104.958734125,31.3750000013656,-43.4753311640868));
#10510=CARTESIAN_POINT('Ctrl Pts',(-74.2170326445434,31.3125000013656,-74.2170326445434));
#10511=CARTESIAN_POINT('Ctrl Pts',(-43.4753311640868,31.2500000013656,-104.958734125));
#10512=CARTESIAN_POINT('Ctrl Pts',(-6.42686888943697E-15,31.1875000013656,
-104.958734125));
#10513=CARTESIAN_POINT('Ctrl Pts',(43.4753311640868,31.1250000013656,-104.958734125));
#10514=CARTESIAN_POINT('Ctrl Pts',(74.2170326445434,31.0625000013656,-74.2170326445434));
#10515=CARTESIAN_POINT('Ctrl Pts',(104.958734125,31.0000000013656,-43.4753311640868));
#10516=CARTESIAN_POINT('Ctrl Pts',(104.958734125,30.9375000013656,-1.28537377788739E-14));
#10517=CARTESIAN_POINT('Ctrl Pts',(104.958734125,30.8750000013656,43.4753311640868));
#10518=CARTESIAN_POINT('Ctrl Pts',(74.2170326445434,30.8125000013656,74.2170326445434));
#10519=CARTESIAN_POINT('Ctrl Pts',(43.4753311640869,30.7500000013656,104.958734125));
#10520=CARTESIAN_POINT('Ctrl Pts',(1.92806066683109E-14,30.6875000013656,
104.958734125));
#10521=CARTESIAN_POINT('Ctrl Pts',(-43.4753311640868,30.6250000013656,104.958734125));
#10522=CARTESIAN_POINT('Ctrl Pts',(-74.2170326445434,30.5625000013656,74.2170326445434));
#10523=CARTESIAN_POINT('Ctrl Pts',(-104.958734125,30.5000000013656,43.4753311640869));
#10524=CARTESIAN_POINT('Ctrl Pts',(-104.958734125,30.4375000013656,0.));
#10525=CARTESIAN_POINT('Ctrl Pts',(-104.958734125,30.3750000013656,-43.4753311640868));
#10526=CARTESIAN_POINT('Ctrl Pts',(-74.2170326445434,30.3125000013656,-74.2170326445434));
#10527=CARTESIAN_POINT('Ctrl Pts',(-43.4753311640868,30.2500000013656,-104.958734125));
#10528=CARTESIAN_POINT('Ctrl Pts',(-6.42686888943697E-15,30.1875000013656,
-104.958734125));
#10529=CARTESIAN_POINT('Ctrl Pts',(43.4753311640868,30.1250000013656,-104.958734125));
#10530=CARTESIAN_POINT('Ctrl Pts',(74.2170326445434,30.0625000013656,-74.2170326445434));
#10531=CARTESIAN_POINT('Ctrl Pts',(104.958734125,30.0000000013656,-43.4753311640868));
#10532=CARTESIAN_POINT('Ctrl Pts',(104.958734125,29.9375000013656,-1.28537377788739E-14));
#10533=CARTESIAN_POINT('Ctrl Pts',(104.958734125,29.8750000013656,43.4753311640868));
#10534=CARTESIAN_POINT('Ctrl Pts',(74.2170326445434,29.8125000013656,74.2170326445434));
#10535=CARTESIAN_POINT('Ctrl Pts',(43.4753311640869,29.7500000013656,104.958734125));
#10536=CARTESIAN_POINT('Ctrl Pts',(1.92806066683109E-14,29.6875000013656,
104.958734125));
#10537=CARTESIAN_POINT('Ctrl Pts',(-43.4753311640868,29.6250000013656,104.958734125));
#10538=CARTESIAN_POINT('Ctrl Pts',(-74.2170326445434,29.5625000013656,74.2170326445434));
#10539=CARTESIAN_POINT('Ctrl Pts',(-104.958734125,29.5000000013656,43.4753311640869));
#10540=CARTESIAN_POINT('Ctrl Pts',(-104.958734125,29.4375000013656,0.));
#10541=CARTESIAN_POINT('Ctrl Pts',(-104.958734125,29.3750000013656,-43.4753311640868));
#10542=CARTESIAN_POINT('Ctrl Pts',(-74.2170326445434,29.3125000013656,-74.2170326445434));
#10543=CARTESIAN_POINT('Ctrl Pts',(-43.4753311640868,29.2500000013656,-104.958734125));
#10544=CARTESIAN_POINT('Ctrl Pts',(-6.42686888943697E-15,29.1875000013656,
-104.958734125));
#10545=CARTESIAN_POINT('Ctrl Pts',(43.4753311640868,29.1250000013656,-104.958734125));
#10546=CARTESIAN_POINT('Ctrl Pts',(74.2170326445434,29.0625000013656,-74.2170326445434));
#10547=CARTESIAN_POINT('Ctrl Pts',(104.958734125,29.0000000013656,-43.4753311640868));
#10548=CARTESIAN_POINT('Ctrl Pts',(104.958734125,28.9375000013656,-1.28537377788739E-14));
#10549=CARTESIAN_POINT('Ctrl Pts',(104.958734125,28.8750000013656,43.4753311640868));
#10550=CARTESIAN_POINT('Ctrl Pts',(74.2170326445434,28.8125000013656,74.2170326445434));
#10551=CARTESIAN_POINT('Ctrl Pts',(43.4753311640869,28.7500000013656,104.958734125));
#10552=CARTESIAN_POINT('Ctrl Pts',(1.92806066683109E-14,28.6875000013656,
104.958734125));
#10553=CARTESIAN_POINT('Ctrl Pts',(-43.4753311640868,28.6250000013656,104.958734125));
#10554=CARTESIAN_POINT('Ctrl Pts',(-74.2170326445434,28.5625000013656,74.2170326445434));
#10555=CARTESIAN_POINT('Ctrl Pts',(-104.958734125,28.5000000013656,43.4753311640869));
#10556=CARTESIAN_POINT('Ctrl Pts',(-104.958734125,28.4375000013656,0.));
#10557=CARTESIAN_POINT('Ctrl Pts',(-104.958734125,28.3750000013656,-43.4753311640868));
#10558=CARTESIAN_POINT('Ctrl Pts',(-74.2170326445434,28.3125000013656,-74.2170326445434));
#10559=CARTESIAN_POINT('Ctrl Pts',(-43.4753311640868,28.2500000013656,-104.958734125));
#10560=CARTESIAN_POINT('Ctrl Pts',(-6.42686888943697E-15,28.1875000013656,
-104.958734125));
#10561=CARTESIAN_POINT('Ctrl Pts',(43.4753311640868,28.1250000013656,-104.958734125));
#10562=CARTESIAN_POINT('Ctrl Pts',(74.2170326445434,28.0625000013656,-74.2170326445434));
#10563=CARTESIAN_POINT('Ctrl Pts',(104.958734125,28.0000000013656,-43.4753311640868));
#10564=CARTESIAN_POINT('Ctrl Pts',(104.958734125,27.9375000013656,-1.28537377788739E-14));
#10565=CARTESIAN_POINT('Ctrl Pts',(104.958734125,27.8750000013656,43.4753311640868));
#10566=CARTESIAN_POINT('Ctrl Pts',(74.2170326445434,27.8125000013656,74.2170326445434));
#10567=CARTESIAN_POINT('Ctrl Pts',(43.4753311640869,27.7500000013656,104.958734125));
#10568=CARTESIAN_POINT('Ctrl Pts',(1.92806066683109E-14,27.6875000013656,
104.958734125));
#10569=CARTESIAN_POINT('Ctrl Pts',(-43.4753311640868,27.6250000013656,104.958734125));
#10570=CARTESIAN_POINT('Ctrl Pts',(-74.2170326445434,27.5625000013656,74.2170326445434));
#10571=CARTESIAN_POINT('Ctrl Pts',(-104.958734125,27.5000000013656,43.4753311640869));
#10572=CARTESIAN_POINT('Ctrl Pts',(-104.958734125,27.4375000013656,0.));
#10573=CARTESIAN_POINT('Ctrl Pts',(-104.958734125,27.3750000013656,-43.4753311640868));
#10574=CARTESIAN_POINT('Ctrl Pts',(-74.2170326445434,27.3125000013656,-74.2170326445434));
#10575=CARTESIAN_POINT('Ctrl Pts',(-43.4753311640868,27.2500000013656,-104.958734125));
#10576=CARTESIAN_POINT('Ctrl Pts',(-6.42686888943697E-15,27.1875000013656,
-104.958734125));
#10577=CARTESIAN_POINT('Ctrl Pts',(43.4753311640868,27.1250000013656,-104.958734125));
#10578=CARTESIAN_POINT('Ctrl Pts',(74.2170326445434,27.0625000013656,-74.2170326445434));
#10579=CARTESIAN_POINT('Ctrl Pts',(104.958734125,27.0000000013656,-43.4753311640868));
#10580=CARTESIAN_POINT('Ctrl Pts',(104.958734125,26.9375000013656,-1.28537377788739E-14));
#10581=CARTESIAN_POINT('Ctrl Pts',(104.958734125,26.8750000013656,43.4753311640868));
#10582=CARTESIAN_POINT('Ctrl Pts',(74.2170326445434,26.8125000013656,74.2170326445434));
#10583=CARTESIAN_POINT('Ctrl Pts',(43.4753311640869,26.7500000013656,104.958734125));
#10584=CARTESIAN_POINT('Ctrl Pts',(1.92806066683109E-14,26.6875000013656,
104.958734125));
#10585=CARTESIAN_POINT('Ctrl Pts',(-43.4753311640868,26.6250000013656,104.958734125));
#10586=CARTESIAN_POINT('Ctrl Pts',(-74.2170326445434,26.5625000013656,74.2170326445434));
#10587=CARTESIAN_POINT('Ctrl Pts',(-104.958734125,26.5000000013656,43.4753311640869));
#10588=CARTESIAN_POINT('Ctrl Pts',(-104.958734125,26.4375000013656,0.));
#10589=CARTESIAN_POINT('Ctrl Pts',(-104.958734125,26.3750000013656,-43.4753311640868));
#10590=CARTESIAN_POINT('Ctrl Pts',(-74.2170326445434,26.3125000013656,-74.2170326445434));
#10591=CARTESIAN_POINT('Ctrl Pts',(-43.4753311640868,26.2500000013656,-104.958734125));
#10592=CARTESIAN_POINT('Ctrl Pts',(-6.42686888943697E-15,26.1875000013656,
-104.958734125));
#10593=CARTESIAN_POINT('Ctrl Pts',(43.4753311640868,26.1250000013656,-104.958734125));
#10594=CARTESIAN_POINT('Ctrl Pts',(74.2170326445434,26.0625000013656,-74.2170326445434));
#10595=CARTESIAN_POINT('Ctrl Pts',(104.958734125,26.0000000013656,-43.4753311640868));
#10596=CARTESIAN_POINT('Ctrl Pts',(104.958734125,25.9375000013656,-1.28537377788739E-14));
#10597=CARTESIAN_POINT('Ctrl Pts',(104.958734125,25.8750000013656,43.4753311640868));
#10598=CARTESIAN_POINT('Ctrl Pts',(74.2170326445434,25.8125000013656,74.2170326445434));
#10599=CARTESIAN_POINT('Ctrl Pts',(43.4753311640869,25.7500000013656,104.958734125));
#10600=CARTESIAN_POINT('Ctrl Pts',(1.92806066683109E-14,25.6875000013656,
104.958734125));
#10601=CARTESIAN_POINT('Ctrl Pts',(-43.4753311640868,25.6250000013656,104.958734125));
#10602=CARTESIAN_POINT('Ctrl Pts',(-74.2170326445434,25.5625000013656,74.2170326445434));
#10603=CARTESIAN_POINT('Ctrl Pts',(-104.958734125,25.5000000013656,43.4753311640869));
#10604=CARTESIAN_POINT('Ctrl Pts',(-104.958734125,25.4375000013656,0.));
#10605=CARTESIAN_POINT('Ctrl Pts',(-104.958734125,25.3750000013656,-43.4753311640868));
#10606=CARTESIAN_POINT('Ctrl Pts',(-74.2170326445434,25.3125000013656,-74.2170326445434));
#10607=CARTESIAN_POINT('Ctrl Pts',(-43.4753311640868,25.2500000013656,-104.958734125));
#10608=CARTESIAN_POINT('Ctrl Pts',(-6.42686888943697E-15,25.1875000013656,
-104.958734125));
#10609=CARTESIAN_POINT('Ctrl Pts',(43.4753311640868,25.1250000013656,-104.958734125));
#10610=CARTESIAN_POINT('Ctrl Pts',(74.2170326445434,25.0625000013656,-74.2170326445434));
#10611=CARTESIAN_POINT('Ctrl Pts',(104.958734125,25.0000000013656,-43.4753311640868));
#10612=CARTESIAN_POINT('Ctrl Pts',(104.958734125,24.9375000013656,-1.28537377788739E-14));
#10613=CARTESIAN_POINT('Ctrl Pts',(104.958734125,24.8750000013656,43.4753311640868));
#10614=CARTESIAN_POINT('Ctrl Pts',(74.2170326445434,24.8125000013656,74.2170326445434));
#10615=CARTESIAN_POINT('Ctrl Pts',(43.4753311640869,24.7500000013656,104.958734125));
#10616=CARTESIAN_POINT('Ctrl Pts',(1.92806066683109E-14,24.6875000013656,
104.958734125));
#10617=CARTESIAN_POINT('Ctrl Pts',(-43.4753311640868,24.6250000013656,104.958734125));
#10618=CARTESIAN_POINT('Ctrl Pts',(-74.2170326445434,24.5625000013656,74.2170326445434));
#10619=CARTESIAN_POINT('Ctrl Pts',(-104.958734125,24.5000000013656,43.4753311640869));
#10620=CARTESIAN_POINT('Ctrl Pts',(-104.958734125,24.4375000013656,0.));
#10621=CARTESIAN_POINT('Ctrl Pts',(-104.958734125,24.3750000013656,-43.4753311640868));
#10622=CARTESIAN_POINT('Ctrl Pts',(-74.2170326445434,24.3125000013656,-74.2170326445434));
#10623=CARTESIAN_POINT('Ctrl Pts',(-43.4753311640868,24.2500000013656,-104.958734125));
#10624=CARTESIAN_POINT('Ctrl Pts',(-6.42686888943697E-15,24.1875000013656,
-104.958734125));
#10625=CARTESIAN_POINT('Ctrl Pts',(43.4753311640868,24.1250000013656,-104.958734125));
#10626=CARTESIAN_POINT('Ctrl Pts',(74.2170326445434,24.0625000013656,-74.2170326445434));
#10627=CARTESIAN_POINT('Ctrl Pts',(104.958734125,24.0000000013656,-43.4753311640868));
#10628=CARTESIAN_POINT('Ctrl Pts',(104.958734125,23.9375000013656,-1.28537377788739E-14));
#10629=CARTESIAN_POINT('Ctrl Pts',(104.958734125,23.8750000013656,43.4753311640868));
#10630=CARTESIAN_POINT('Ctrl Pts',(74.2170326445434,23.8125000013656,74.2170326445434));
#10631=CARTESIAN_POINT('Ctrl Pts',(43.4753311640869,23.7500000013656,104.958734125));
#10632=CARTESIAN_POINT('Ctrl Pts',(1.92806066683109E-14,23.6875000013656,
104.958734125));
#10633=CARTESIAN_POINT('Ctrl Pts',(-43.4753311640868,23.6250000013656,104.958734125));
#10634=CARTESIAN_POINT('Ctrl Pts',(-74.2170326445434,23.5625000013656,74.2170326445434));
#10635=CARTESIAN_POINT('Ctrl Pts',(-104.958734125,23.5000000013656,43.4753311640869));
#10636=CARTESIAN_POINT('Ctrl Pts',(-104.958734125,23.4375000013656,0.));
#10637=CARTESIAN_POINT('Ctrl Pts',(-104.958734125,23.3750000013656,-43.4753311640868));
#10638=CARTESIAN_POINT('Ctrl Pts',(-74.2170326445434,23.3125000013656,-74.2170326445434));
#10639=CARTESIAN_POINT('Ctrl Pts',(-43.4753311640868,23.2500000013656,-104.958734125));
#10640=CARTESIAN_POINT('Ctrl Pts',(-6.42686888943697E-15,23.1875000013656,
-104.958734125));
#10641=CARTESIAN_POINT('Ctrl Pts',(43.4753311640868,23.1250000013656,-104.958734125));
#10642=CARTESIAN_POINT('Ctrl Pts',(74.2170326445434,23.0625000013656,-74.2170326445434));
#10643=CARTESIAN_POINT('Ctrl Pts',(104.958734125,23.0000000013656,-43.4753311640868));
#10644=CARTESIAN_POINT('Ctrl Pts',(104.958734125,22.9375000013656,-1.28537377788739E-14));
#10645=CARTESIAN_POINT('Ctrl Pts',(104.958734125,22.8750000013656,43.4753311640868));
#10646=CARTESIAN_POINT('Ctrl Pts',(74.2170326445434,22.8125000013656,74.2170326445434));
#10647=CARTESIAN_POINT('Ctrl Pts',(43.4753311640869,22.7500000013656,104.958734125));
#10648=CARTESIAN_POINT('Ctrl Pts',(1.92806066683109E-14,22.6875000013656,
104.958734125));
#10649=CARTESIAN_POINT('Ctrl Pts',(-43.4753311640868,22.6250000013656,104.958734125));
#10650=CARTESIAN_POINT('Ctrl Pts',(-74.2170326445434,22.5625000013656,74.2170326445434));
#10651=CARTESIAN_POINT('Ctrl Pts',(-104.958734125,22.5000000013656,43.4753311640869));
#10652=CARTESIAN_POINT('Ctrl Pts',(-104.958734125,22.4375000013656,0.));
#10653=CARTESIAN_POINT('Ctrl Pts',(-104.958734125,22.3750000013656,-43.4753311640868));
#10654=CARTESIAN_POINT('Ctrl Pts',(-74.2170326445434,22.3125000013656,-74.2170326445434));
#10655=CARTESIAN_POINT('Ctrl Pts',(-43.4753311640868,22.2500000013656,-104.958734125));
#10656=CARTESIAN_POINT('Ctrl Pts',(-6.42686888943697E-15,22.1875000013656,
-104.958734125));
#10657=CARTESIAN_POINT('Ctrl Pts',(43.4753311640868,22.1250000013656,-104.958734125));
#10658=CARTESIAN_POINT('Ctrl Pts',(74.2170326445434,22.0625000013656,-74.2170326445434));
#10659=CARTESIAN_POINT('Ctrl Pts',(104.958734125,22.0000000013656,-43.4753311640868));
#10660=CARTESIAN_POINT('Ctrl Pts',(104.958734125,21.9375000013656,-1.28537377788739E-14));
#10661=CARTESIAN_POINT('Ctrl Pts',(104.958734125,21.8750000013656,43.4753311640868));
#10662=CARTESIAN_POINT('Ctrl Pts',(74.2170326445434,21.8125000013656,74.2170326445434));
#10663=CARTESIAN_POINT('Ctrl Pts',(43.4753311640869,21.7500000013656,104.958734125));
#10664=CARTESIAN_POINT('Ctrl Pts',(1.92806066683109E-14,21.6875000013656,
104.958734125));
#10665=CARTESIAN_POINT('Ctrl Pts',(-43.4753311640868,21.6250000013656,104.958734125));
#10666=CARTESIAN_POINT('Ctrl Pts',(-74.2170326445434,21.5625000013656,74.2170326445434));
#10667=CARTESIAN_POINT('Ctrl Pts',(-104.958734125,21.5000000013656,43.4753311640869));
#10668=CARTESIAN_POINT('Ctrl Pts',(-104.958734125,21.4375000013656,0.));
#10669=CARTESIAN_POINT('Ctrl Pts',(-104.958734125,21.3750000013656,-43.4753311640868));
#10670=CARTESIAN_POINT('Ctrl Pts',(-74.2170326445434,21.3125000013656,-74.2170326445434));
#10671=CARTESIAN_POINT('Ctrl Pts',(-43.4753311640868,21.2500000013656,-104.958734125));
#10672=CARTESIAN_POINT('Ctrl Pts',(-6.42686888943697E-15,21.1875000013656,
-104.958734125));
#10673=CARTESIAN_POINT('Ctrl Pts',(43.4753311640868,21.1250000013656,-104.958734125));
#10674=CARTESIAN_POINT('Ctrl Pts',(74.2170326445434,21.0625000013656,-74.2170326445434));
#10675=CARTESIAN_POINT('Ctrl Pts',(104.958734125,21.0000000013656,-43.4753311640868));
#10676=CARTESIAN_POINT('Ctrl Pts',(104.958734125,20.9375000013656,-1.28537377788739E-14));
#10677=CARTESIAN_POINT('Ctrl Pts',(104.958734125,20.8750000013656,43.4753311640868));
#10678=CARTESIAN_POINT('Ctrl Pts',(74.2170326445434,20.8125000013656,74.2170326445434));
#10679=CARTESIAN_POINT('Ctrl Pts',(43.4753311640869,20.7500000013656,104.958734125));
#10680=CARTESIAN_POINT('Ctrl Pts',(1.92806066683109E-14,20.6875000013656,
104.958734125));
#10681=CARTESIAN_POINT('Ctrl Pts',(-43.4753311640868,20.6250000013656,104.958734125));
#10682=CARTESIAN_POINT('Ctrl Pts',(-74.2170326445434,20.5625000013656,74.2170326445434));
#10683=CARTESIAN_POINT('Ctrl Pts',(-104.958734125,20.5000000013656,43.4753311640869));
#10684=CARTESIAN_POINT('Ctrl Pts',(-104.958734125,20.4375000013656,0.));
#10685=CARTESIAN_POINT('Ctrl Pts',(-104.958734125,20.3750000013656,-43.4753311640868));
#10686=CARTESIAN_POINT('Ctrl Pts',(-74.2170326445434,20.3125000013656,-74.2170326445434));
#10687=CARTESIAN_POINT('Ctrl Pts',(-43.4753311640868,20.2500000013656,-104.958734125));
#10688=CARTESIAN_POINT('Ctrl Pts',(-6.42686888943697E-15,20.1875000013656,
-104.958734125));
#10689=CARTESIAN_POINT('Ctrl Pts',(43.4753311640868,20.1250000013656,-104.958734125));
#10690=CARTESIAN_POINT('Ctrl Pts',(74.2170326445434,20.0625000013656,-74.2170326445434));
#10691=CARTESIAN_POINT('Ctrl Pts',(104.958734125,20.0000000013656,-43.4753311640868));
#10692=CARTESIAN_POINT('Ctrl Pts',(104.958734125,19.9375000013656,-1.28537377788739E-14));
#10693=CARTESIAN_POINT('Ctrl Pts',(104.958734125,19.8750000013656,43.4753311640868));
#10694=CARTESIAN_POINT('Ctrl Pts',(74.2170326445434,19.8125000013656,74.2170326445434));
#10695=CARTESIAN_POINT('Ctrl Pts',(43.4753311640869,19.7500000013656,104.958734125));
#10696=CARTESIAN_POINT('Ctrl Pts',(1.92806066683109E-14,19.6875000013656,
104.958734125));
#10697=CARTESIAN_POINT('Ctrl Pts',(-43.4753311640868,19.6250000013656,104.958734125));
#10698=CARTESIAN_POINT('Ctrl Pts',(-74.2170326445434,19.5625000013656,74.2170326445434));
#10699=CARTESIAN_POINT('Ctrl Pts',(-104.958734125,19.5000000013656,43.4753311640869));
#10700=CARTESIAN_POINT('Ctrl Pts',(-104.958734125,19.4375000013656,0.));
#10701=CARTESIAN_POINT('Ctrl Pts',(-104.958734125,19.3750000013656,-43.4753311640868));
#10702=CARTESIAN_POINT('Ctrl Pts',(-74.2170326445434,19.3125000013656,-74.2170326445434));
#10703=CARTESIAN_POINT('Ctrl Pts',(-43.4753311640868,19.2500000013656,-104.958734125));
#10704=CARTESIAN_POINT('Ctrl Pts',(-6.42686888943697E-15,19.1875000013656,
-104.958734125));
#10705=CARTESIAN_POINT('Ctrl Pts',(43.4753311640868,19.1250000013656,-104.958734125));
#10706=CARTESIAN_POINT('Ctrl Pts',(74.2170326445434,19.0625000013656,-74.2170326445434));
#10707=CARTESIAN_POINT('Ctrl Pts',(104.958734125,19.0000000013656,-43.4753311640868));
#10708=CARTESIAN_POINT('Ctrl Pts',(104.958734125,18.9375000013656,-1.28537377788739E-14));
#10709=CARTESIAN_POINT('Ctrl Pts',(104.958734125,18.8750000013656,43.4753311640868));
#10710=CARTESIAN_POINT('Ctrl Pts',(74.2170326445434,18.8125000013656,74.2170326445434));
#10711=CARTESIAN_POINT('Ctrl Pts',(43.4753311640869,18.7500000013656,104.958734125));
#10712=CARTESIAN_POINT('Ctrl Pts',(1.92806066683109E-14,18.6875000013656,
104.958734125));
#10713=CARTESIAN_POINT('Ctrl Pts',(-43.4753311640868,18.6250000013656,104.958734125));
#10714=CARTESIAN_POINT('Ctrl Pts',(-74.2170326445434,18.5625000013656,74.2170326445434));
#10715=CARTESIAN_POINT('Ctrl Pts',(-104.958734125,18.5000000013656,43.4753311640869));
#10716=CARTESIAN_POINT('Ctrl Pts',(-104.958734125,18.4375000013656,0.));
#10717=CARTESIAN_POINT('Ctrl Pts',(-104.958734125,18.3750000013656,-43.4753311640868));
#10718=CARTESIAN_POINT('Ctrl Pts',(-74.2170326445434,18.3125000013656,-74.2170326445434));
#10719=CARTESIAN_POINT('Ctrl Pts',(-43.4753311640868,18.2500000013656,-104.958734125));
#10720=CARTESIAN_POINT('Ctrl Pts',(-6.42686888943697E-15,18.1875000013656,
-104.958734125));
#10721=CARTESIAN_POINT('Ctrl Pts',(43.4753311640868,18.1250000013656,-104.958734125));
#10722=CARTESIAN_POINT('Ctrl Pts',(74.2170326445434,18.0625000013656,-74.2170326445434));
#10723=CARTESIAN_POINT('Ctrl Pts',(104.958734125,18.0000000013656,-43.4753311640868));
#10724=CARTESIAN_POINT('Ctrl Pts',(104.958734125,17.9375000013656,-1.28537377788739E-14));
#10725=CARTESIAN_POINT('Ctrl Pts',(104.958734125,17.8750000013656,43.4753311640868));
#10726=CARTESIAN_POINT('Ctrl Pts',(74.2170326445434,17.8125000013656,74.2170326445434));
#10727=CARTESIAN_POINT('Ctrl Pts',(43.4753311640869,17.7500000013656,104.958734125));
#10728=CARTESIAN_POINT('Ctrl Pts',(1.92806066683109E-14,17.6875000013656,
104.958734125));
#10729=CARTESIAN_POINT('Ctrl Pts',(-43.4753311640868,17.6250000013656,104.958734125));
#10730=CARTESIAN_POINT('Ctrl Pts',(-74.2170326445434,17.5625000013656,74.2170326445434));
#10731=CARTESIAN_POINT('Ctrl Pts',(-104.958734125,17.5000000013656,43.4753311640869));
#10732=CARTESIAN_POINT('Ctrl Pts',(-104.958734125,17.4375000013656,0.));
#10733=CARTESIAN_POINT('Ctrl Pts',(-104.958734125,17.3750000013656,-43.4753311640868));
#10734=CARTESIAN_POINT('Ctrl Pts',(-74.2170326445434,17.3125000013656,-74.2170326445434));
#10735=CARTESIAN_POINT('Ctrl Pts',(-43.4753311640868,17.2500000013656,-104.958734125));
#10736=CARTESIAN_POINT('Ctrl Pts',(-6.42686888943697E-15,17.1875000013656,
-104.958734125));
#10737=CARTESIAN_POINT('Ctrl Pts',(43.4753311640868,17.1250000013656,-104.958734125));
#10738=CARTESIAN_POINT('Ctrl Pts',(74.2170326445434,17.0625000013656,-74.2170326445434));
#10739=CARTESIAN_POINT('Ctrl Pts',(104.958734125,17.0000000013656,-43.4753311640868));
#10740=CARTESIAN_POINT('Ctrl Pts',(104.958734125,16.9375000013656,-1.28537377788739E-14));
#10741=CARTESIAN_POINT('Ctrl Pts',(104.958734125,16.8750000013656,43.4753311640868));
#10742=CARTESIAN_POINT('Ctrl Pts',(74.2170326445434,16.8125000013656,74.2170326445434));
#10743=CARTESIAN_POINT('Ctrl Pts',(43.4753311640869,16.7500000013656,104.958734125));
#10744=CARTESIAN_POINT('Ctrl Pts',(1.92806066683109E-14,16.6875000013656,
104.958734125));
#10745=CARTESIAN_POINT('Ctrl Pts',(-43.4753311640868,16.6250000013656,104.958734125));
#10746=CARTESIAN_POINT('Ctrl Pts',(-74.2170326445434,16.5625000013656,74.2170326445434));
#10747=CARTESIAN_POINT('Ctrl Pts',(-104.958734125,16.5000000013656,43.4753311640869));
#10748=CARTESIAN_POINT('Ctrl Pts',(-104.958734125,16.4375000013656,0.));
#10749=CARTESIAN_POINT('Ctrl Pts',(-104.958734125,16.3750000013656,-43.4753311640868));
#10750=CARTESIAN_POINT('Ctrl Pts',(-74.2170326445434,16.3125000013656,-74.2170326445434));
#10751=CARTESIAN_POINT('Ctrl Pts',(-43.4753311640868,16.2500000013656,-104.958734125));
#10752=CARTESIAN_POINT('Ctrl Pts',(-6.42686888943697E-15,16.1875000013656,
-104.958734125));
#10753=CARTESIAN_POINT('Ctrl Pts',(43.4753311640868,16.1250000013656,-104.958734125));
#10754=CARTESIAN_POINT('Ctrl Pts',(74.2170326445434,16.0625000013656,-74.2170326445434));
#10755=CARTESIAN_POINT('Ctrl Pts',(104.958734125,16.0000000013656,-43.4753311640868));
#10756=CARTESIAN_POINT('Ctrl Pts',(104.958734125,15.9375000013656,-1.28537377788739E-14));
#10757=CARTESIAN_POINT('Ctrl Pts',(104.958734125,15.8750000013656,43.4753311640868));
#10758=CARTESIAN_POINT('Ctrl Pts',(74.2170326445434,15.8125000013656,74.2170326445434));
#10759=CARTESIAN_POINT('Ctrl Pts',(43.4753311640869,15.7500000013656,104.958734125));
#10760=CARTESIAN_POINT('Ctrl Pts',(1.92806066683109E-14,15.6875000013656,
104.958734125));
#10761=CARTESIAN_POINT('Ctrl Pts',(-43.4753311640868,15.6250000013656,104.958734125));
#10762=CARTESIAN_POINT('Ctrl Pts',(-74.2170326445434,15.5625000013656,74.2170326445434));
#10763=CARTESIAN_POINT('Ctrl Pts',(-104.958734125,15.5000000013656,43.4753311640869));
#10764=CARTESIAN_POINT('Ctrl Pts',(-104.958734125,15.4375000013656,0.));
#10765=CARTESIAN_POINT('Ctrl Pts',(-104.958734125,15.3750000013656,-43.4753311640868));
#10766=CARTESIAN_POINT('Ctrl Pts',(-74.2170326445434,15.3125000013656,-74.2170326445434));
#10767=CARTESIAN_POINT('Ctrl Pts',(-43.4753311640868,15.2500000013656,-104.958734125));
#10768=CARTESIAN_POINT('Ctrl Pts',(-6.42686888943697E-15,15.1875000013656,
-104.958734125));
#10769=CARTESIAN_POINT('Ctrl Pts',(43.4753311640868,15.1250000013656,-104.958734125));
#10770=CARTESIAN_POINT('Ctrl Pts',(74.2170326445434,15.0625000013656,-74.2170326445434));
#10771=CARTESIAN_POINT('Ctrl Pts',(104.958734125,15.0000000013656,-43.4753311640868));
#10772=CARTESIAN_POINT('Ctrl Pts',(104.958734125,14.9375000013656,-1.28537377788739E-14));
#10773=CARTESIAN_POINT('Ctrl Pts',(104.958734125,14.8750000013656,43.4753311640868));
#10774=CARTESIAN_POINT('Ctrl Pts',(74.2170326445434,14.8125000013656,74.2170326445434));
#10775=CARTESIAN_POINT('Ctrl Pts',(43.4753311640869,14.7500000013656,104.958734125));
#10776=CARTESIAN_POINT('Ctrl Pts',(1.92806066683109E-14,14.6875000013656,
104.958734125));
#10777=CARTESIAN_POINT('Ctrl Pts',(-43.4753311640868,14.6250000013656,104.958734125));
#10778=CARTESIAN_POINT('Ctrl Pts',(-74.2170326445434,14.5625000013656,74.2170326445434));
#10779=CARTESIAN_POINT('Ctrl Pts',(-104.958734125,14.5000000013656,43.4753311640869));
#10780=CARTESIAN_POINT('Ctrl Pts',(-104.958734125,14.4375000013656,0.));
#10781=CARTESIAN_POINT('Ctrl Pts',(-104.958734125,14.3750000013656,-43.4753311640868));
#10782=CARTESIAN_POINT('Ctrl Pts',(-74.2170326445434,14.3125000013656,-74.2170326445434));
#10783=CARTESIAN_POINT('Ctrl Pts',(-43.4753311640868,14.2500000013656,-104.958734125));
#10784=CARTESIAN_POINT('Ctrl Pts',(-6.42686888943697E-15,14.1875000013656,
-104.958734125));
#10785=CARTESIAN_POINT('Ctrl Pts',(43.4753311640868,14.1250000013656,-104.958734125));
#10786=CARTESIAN_POINT('Ctrl Pts',(74.2170326445434,14.0625000013656,-74.2170326445434));
#10787=CARTESIAN_POINT('Ctrl Pts',(104.958734125,14.0000000013656,-43.4753311640868));
#10788=CARTESIAN_POINT('Ctrl Pts',(104.958734125,13.9375000013656,-1.28537377788739E-14));
#10789=CARTESIAN_POINT('Ctrl Pts',(104.958734125,13.8750000013656,43.4753311640868));
#10790=CARTESIAN_POINT('Ctrl Pts',(74.2170326445434,13.8125000013656,74.2170326445434));
#10791=CARTESIAN_POINT('Ctrl Pts',(43.4753311640869,13.7500000013656,104.958734125));
#10792=CARTESIAN_POINT('Ctrl Pts',(1.92806066683109E-14,13.6875000013656,
104.958734125));
#10793=CARTESIAN_POINT('Ctrl Pts',(-43.4753311640868,13.6250000013656,104.958734125));
#10794=CARTESIAN_POINT('Ctrl Pts',(-74.2170326445434,13.5625000013656,74.2170326445434));
#10795=CARTESIAN_POINT('Ctrl Pts',(-104.958734125,13.5000000013656,43.4753311640869));
#10796=CARTESIAN_POINT('Ctrl Pts',(-104.958734125,13.4375000013656,0.));
#10797=CARTESIAN_POINT('Ctrl Pts',(-104.958734125,13.3750000013656,-43.4753311640868));
#10798=CARTESIAN_POINT('Ctrl Pts',(-74.2170326445434,13.3125000013656,-74.2170326445434));
#10799=CARTESIAN_POINT('Ctrl Pts',(-43.4753311640868,13.2500000013656,-104.958734125));
#10800=CARTESIAN_POINT('Ctrl Pts',(-6.42686888943697E-15,13.1875000013656,
-104.958734125));
#10801=CARTESIAN_POINT('Ctrl Pts',(43.4753311640868,13.1250000013656,-104.958734125));
#10802=CARTESIAN_POINT('Ctrl Pts',(74.2170326445434,13.0625000013656,-74.2170326445434));
#10803=CARTESIAN_POINT('Ctrl Pts',(104.958734125,13.0000000013656,-43.4753311640868));
#10804=CARTESIAN_POINT('Ctrl Pts',(104.958734125,12.9375000013656,-1.28537377788739E-14));
#10805=CARTESIAN_POINT('Ctrl Pts',(104.958734125,12.8750000013656,43.4753311640868));
#10806=CARTESIAN_POINT('Ctrl Pts',(74.2170326445434,12.8125000013656,74.2170326445434));
#10807=CARTESIAN_POINT('Ctrl Pts',(43.4753311640869,12.7500000013656,104.958734125));
#10808=CARTESIAN_POINT('Ctrl Pts',(1.92806066683109E-14,12.6875000013656,
104.958734125));
#10809=CARTESIAN_POINT('Ctrl Pts',(-43.4753311640868,12.6250000013656,104.958734125));
#10810=CARTESIAN_POINT('Ctrl Pts',(-74.2170326445434,12.5625000013656,74.2170326445434));
#10811=CARTESIAN_POINT('Ctrl Pts',(-104.958734125,12.5000000013656,43.4753311640869));
#10812=CARTESIAN_POINT('Ctrl Pts',(-104.958734125,12.4375000013656,0.));
#10813=CARTESIAN_POINT('Ctrl Pts',(-104.958734125,12.3750000013656,-43.4753311640868));
#10814=CARTESIAN_POINT('Ctrl Pts',(-74.2170326445434,12.3125000013656,-74.2170326445434));
#10815=CARTESIAN_POINT('Ctrl Pts',(-43.4753311640868,12.2500000013656,-104.958734125));
#10816=CARTESIAN_POINT('Ctrl Pts',(-6.42686888943697E-15,12.1875000013656,
-104.958734125));
#10817=CARTESIAN_POINT('Ctrl Pts',(43.4753311640868,12.1250000013656,-104.958734125));
#10818=CARTESIAN_POINT('Ctrl Pts',(74.2170326445434,12.0625000013656,-74.2170326445434));
#10819=CARTESIAN_POINT('Ctrl Pts',(104.958734125,12.0000000013656,-43.4753311640868));
#10820=CARTESIAN_POINT('Ctrl Pts',(104.958734125,11.9375000013656,-1.28537377788739E-14));
#10821=CARTESIAN_POINT('Ctrl Pts',(104.958734125,11.8750000013656,43.4753311640868));
#10822=CARTESIAN_POINT('Ctrl Pts',(74.2170326445434,11.8125000013656,74.2170326445434));
#10823=CARTESIAN_POINT('Ctrl Pts',(43.4753311640869,11.7500000013656,104.958734125));
#10824=CARTESIAN_POINT('Ctrl Pts',(1.92806066683109E-14,11.6875000013656,
104.958734125));
#10825=CARTESIAN_POINT('Ctrl Pts',(-43.4753311640868,11.6250000013656,104.958734125));
#10826=CARTESIAN_POINT('Ctrl Pts',(-74.2170326445434,11.5625000013656,74.2170326445434));
#10827=CARTESIAN_POINT('Ctrl Pts',(-104.958734125,11.5000000013656,43.4753311640869));
#10828=CARTESIAN_POINT('Ctrl Pts',(-104.958734125,11.4375000013656,0.));
#10829=CARTESIAN_POINT('Ctrl Pts',(-104.958734125,11.3750000013656,-43.4753311640868));
#10830=CARTESIAN_POINT('Ctrl Pts',(-74.2170326445434,11.3125000013656,-74.2170326445434));
#10831=CARTESIAN_POINT('Ctrl Pts',(-43.4753311640868,11.2500000013656,-104.958734125));
#10832=CARTESIAN_POINT('Ctrl Pts',(-6.42686888943697E-15,11.1875000013656,
-104.958734125));
#10833=CARTESIAN_POINT('Ctrl Pts',(43.4753311640868,11.1250000013656,-104.958734125));
#10834=CARTESIAN_POINT('Ctrl Pts',(74.2170326445434,11.0625000013656,-74.2170326445434));
#10835=CARTESIAN_POINT('Ctrl Pts',(104.958734125,11.0000000013656,-43.4753311640868));
#10836=CARTESIAN_POINT('Ctrl Pts',(104.958734125,10.9375000013656,-1.28537377788739E-14));
#10837=CARTESIAN_POINT('Ctrl Pts',(104.958734125,10.8750000013656,43.4753311640868));
#10838=CARTESIAN_POINT('Ctrl Pts',(74.2170326445434,10.8125000013656,74.2170326445434));
#10839=CARTESIAN_POINT('Ctrl Pts',(43.4753311640869,10.7500000013656,104.958734125));
#10840=CARTESIAN_POINT('Ctrl Pts',(1.92806066683109E-14,10.6875000013656,
104.958734125));
#10841=CARTESIAN_POINT('Ctrl Pts',(-43.4753311640868,10.6250000013656,104.958734125));
#10842=CARTESIAN_POINT('Ctrl Pts',(-74.2170326445434,10.5625000013656,74.2170326445434));
#10843=CARTESIAN_POINT('Ctrl Pts',(-104.958734125,10.5000000013656,43.4753311640869));
#10844=CARTESIAN_POINT('Ctrl Pts',(-104.958734125,10.4375000013656,0.));
#10845=CARTESIAN_POINT('Ctrl Pts',(-104.958734125,10.3750000013656,-43.4753311640868));
#10846=CARTESIAN_POINT('Ctrl Pts',(-74.2170326445434,10.3125000013656,-74.2170326445434));
#10847=CARTESIAN_POINT('Ctrl Pts',(-43.4753311640868,10.2500000013656,-104.958734125));
#10848=CARTESIAN_POINT('Ctrl Pts',(-6.42686888943697E-15,10.1875000013656,
-104.958734125));
#10849=CARTESIAN_POINT('Ctrl Pts',(43.4753311640868,10.1250000013656,-104.958734125));
#10850=CARTESIAN_POINT('Ctrl Pts',(74.2170326445434,10.0625000013656,-74.2170326445434));
#10851=CARTESIAN_POINT('Ctrl Pts',(104.958734125,10.0000000013656,-43.4753311640868));
#10852=CARTESIAN_POINT('Ctrl Pts',(104.958734125,9.93750000136558,-1.28537377788739E-14));
#10853=CARTESIAN_POINT('Ctrl Pts',(104.958734125,9.87500000136558,43.4753311640868));
#10854=CARTESIAN_POINT('Ctrl Pts',(74.2170326445434,9.81250000136558,74.2170326445434));
#10855=CARTESIAN_POINT('Ctrl Pts',(43.4753311640869,9.75000000136558,104.958734125));
#10856=CARTESIAN_POINT('Ctrl Pts',(1.92806066683109E-14,9.68750000136558,
104.958734125));
#10857=CARTESIAN_POINT('Ctrl Pts',(-43.4753311640868,9.62500000136558,104.958734125));
#10858=CARTESIAN_POINT('Ctrl Pts',(-74.2170326445434,9.56250000136558,74.2170326445434));
#10859=CARTESIAN_POINT('Ctrl Pts',(-104.958734125,9.50000000136558,43.4753311640869));
#10860=CARTESIAN_POINT('Ctrl Pts',(-104.958734125,9.43750000136558,0.));
#10861=CARTESIAN_POINT('Ctrl Pts',(-104.958734125,9.37500000136558,-43.4753311640868));
#10862=CARTESIAN_POINT('Ctrl Pts',(-74.2170326445434,9.31250000136558,-74.2170326445434));
#10863=CARTESIAN_POINT('Ctrl Pts',(-43.4753311640868,9.25000000136558,-104.958734125));
#10864=CARTESIAN_POINT('Ctrl Pts',(-6.42686888943697E-15,9.18750000136558,
-104.958734125));
#10865=CARTESIAN_POINT('Ctrl Pts',(43.4753311640868,9.12500000136558,-104.958734125));
#10866=CARTESIAN_POINT('Ctrl Pts',(74.2170326445434,9.06250000136558,-74.2170326445434));
#10867=CARTESIAN_POINT('Ctrl Pts',(104.958734125,9.00000000136558,-43.4753311640868));
#10868=CARTESIAN_POINT('Ctrl Pts',(104.958734125,8.93750000136558,-1.28537377788739E-14));
#10869=CARTESIAN_POINT('Ctrl Pts',(104.958734125,8.87500000136558,43.4753311640868));
#10870=CARTESIAN_POINT('Ctrl Pts',(74.2170326445434,8.81250000136558,74.2170326445434));
#10871=CARTESIAN_POINT('Ctrl Pts',(43.4753311640869,8.75000000136558,104.958734125));
#10872=CARTESIAN_POINT('Ctrl Pts',(1.92806066683109E-14,8.68750000136558,
104.958734125));
#10873=CARTESIAN_POINT('Ctrl Pts',(-43.4753311640868,8.62500000136558,104.958734125));
#10874=CARTESIAN_POINT('Ctrl Pts',(-74.2170326445434,8.56250000136558,74.2170326445434));
#10875=CARTESIAN_POINT('Ctrl Pts',(-104.958734125,8.50000000136558,43.4753311640869));
#10876=CARTESIAN_POINT('Ctrl Pts',(-104.958734125,8.43750000136558,0.));
#10877=CARTESIAN_POINT('Ctrl Pts',(-104.958734125,8.37500000136558,-43.4753311640868));
#10878=CARTESIAN_POINT('Ctrl Pts',(-74.2170326445434,8.31250000136558,-74.2170326445434));
#10879=CARTESIAN_POINT('Ctrl Pts',(-43.4753311640868,8.25000000136558,-104.958734125));
#10880=CARTESIAN_POINT('Ctrl Pts',(-6.42686888943697E-15,8.18750000136558,
-104.958734125));
#10881=CARTESIAN_POINT('Ctrl Pts',(43.4753311640868,8.12500000136558,-104.958734125));
#10882=CARTESIAN_POINT('Ctrl Pts',(74.2170326445434,8.06250000136558,-74.2170326445434));
#10883=CARTESIAN_POINT('Ctrl Pts',(104.958734125,8.00000000136558,-43.4753311640868));
#10884=CARTESIAN_POINT('Ctrl Pts',(104.958734125,7.93750000136558,-1.28537377788739E-14));
#10885=CARTESIAN_POINT('Ctrl Pts',(104.958734125,7.87500000136558,43.4753311640868));
#10886=CARTESIAN_POINT('Ctrl Pts',(74.2170326445434,7.81250000136558,74.2170326445434));
#10887=CARTESIAN_POINT('Ctrl Pts',(43.4753311640869,7.75000000136558,104.958734125));
#10888=CARTESIAN_POINT('Ctrl Pts',(1.92806066683109E-14,7.68750000136558,
104.958734125));
#10889=CARTESIAN_POINT('Ctrl Pts',(-43.4753311640868,7.62500000136558,104.958734125));
#10890=CARTESIAN_POINT('Ctrl Pts',(-74.2170326445434,7.56250000136558,74.2170326445434));
#10891=CARTESIAN_POINT('Ctrl Pts',(-104.958734125,7.50000000136558,43.4753311640869));
#10892=CARTESIAN_POINT('Ctrl Pts',(-104.958734125,7.43750000136558,0.));
#10893=CARTESIAN_POINT('Ctrl Pts',(-104.958734125,7.37500000136558,-43.4753311640868));
#10894=CARTESIAN_POINT('Ctrl Pts',(-74.2170326445434,7.31250000136558,-74.2170326445434));
#10895=CARTESIAN_POINT('Ctrl Pts',(-43.4753311640868,7.25000000136558,-104.958734125));
#10896=CARTESIAN_POINT('Ctrl Pts',(-6.42686888943697E-15,7.18750000136558,
-104.958734125));
#10897=CARTESIAN_POINT('Ctrl Pts',(43.4753311640868,7.12500000136558,-104.958734125));
#10898=CARTESIAN_POINT('Ctrl Pts',(74.2170326445434,7.06250000136558,-74.2170326445434));
#10899=CARTESIAN_POINT('Ctrl Pts',(104.958734125,7.00000000136558,-43.4753311640868));
#10900=CARTESIAN_POINT('Ctrl Pts',(104.958734125,6.93750000136558,-1.28537377788739E-14));
#10901=CARTESIAN_POINT('Ctrl Pts',(104.958734125,6.87500000136558,43.4753311640868));
#10902=CARTESIAN_POINT('Ctrl Pts',(74.2170326445434,6.81250000136558,74.2170326445434));
#10903=CARTESIAN_POINT('Ctrl Pts',(43.4753311640869,6.75000000136558,104.958734125));
#10904=CARTESIAN_POINT('Ctrl Pts',(1.92806066683109E-14,6.68750000136558,
104.958734125));
#10905=CARTESIAN_POINT('Ctrl Pts',(-43.4753311640868,6.62500000136558,104.958734125));
#10906=CARTESIAN_POINT('Ctrl Pts',(-74.2170326445434,6.56250000136558,74.2170326445434));
#10907=CARTESIAN_POINT('Ctrl Pts',(-104.958734125,6.50000000136558,43.4753311640869));
#10908=CARTESIAN_POINT('Ctrl Pts',(-104.958734125,6.43750000136558,0.));
#10909=CARTESIAN_POINT('Ctrl Pts',(-104.958734125,6.37500000136558,-43.4753311640868));
#10910=CARTESIAN_POINT('Ctrl Pts',(-74.2170326445434,6.31250000136558,-74.2170326445434));
#10911=CARTESIAN_POINT('Ctrl Pts',(-43.4753311640868,6.25000000136558,-104.958734125));
#10912=CARTESIAN_POINT('Ctrl Pts',(-6.42686888943697E-15,6.18750000136558,
-104.958734125));
#10913=CARTESIAN_POINT('Ctrl Pts',(43.4753311640868,6.12500000136558,-104.958734125));
#10914=CARTESIAN_POINT('Ctrl Pts',(74.2170326445434,6.06250000136558,-74.2170326445434));
#10915=CARTESIAN_POINT('Ctrl Pts',(104.958734125,6.00000000136558,-43.4753311640868));
#10916=CARTESIAN_POINT('Ctrl Pts',(104.958734125,5.93750000136558,-1.28537377788739E-14));
#10917=CARTESIAN_POINT('Ctrl Pts',(104.958734125,5.87500000136558,43.4753311640868));
#10918=CARTESIAN_POINT('Ctrl Pts',(74.2170326445434,5.81250000136558,74.2170326445434));
#10919=CARTESIAN_POINT('Ctrl Pts',(43.4753311640869,5.75000000136558,104.958734125));
#10920=CARTESIAN_POINT('Ctrl Pts',(1.92806066683109E-14,5.68750000136558,
104.958734125));
#10921=CARTESIAN_POINT('Ctrl Pts',(-43.4753311640868,5.62500000136558,104.958734125));
#10922=CARTESIAN_POINT('Ctrl Pts',(-74.2170326445434,5.56250000136558,74.2170326445434));
#10923=CARTESIAN_POINT('Ctrl Pts',(-104.958734125,5.50000000136558,43.4753311640869));
#10924=CARTESIAN_POINT('Ctrl Pts',(-104.958734125,5.43750000136559,0.));
#10925=CARTESIAN_POINT('Ctrl Pts',(-104.958734125,5.37500000136559,-43.4753311640868));
#10926=CARTESIAN_POINT('Ctrl Pts',(-74.2170326445434,5.31250000136558,-74.2170326445434));
#10927=CARTESIAN_POINT('Ctrl Pts',(-43.4753311640868,5.25000000136559,-104.958734125));
#10928=CARTESIAN_POINT('Ctrl Pts',(-6.42686888943697E-15,5.18750000136559,
-104.958734125));
#10929=CARTESIAN_POINT('Ctrl Pts',(43.4753311640868,5.12500000136559,-104.958734125));
#10930=CARTESIAN_POINT('Ctrl Pts',(74.2170326445434,5.06250000136559,-74.2170326445434));
#10931=CARTESIAN_POINT('Ctrl Pts',(104.958734125,5.00000000136558,-43.4753311640868));
#10932=CARTESIAN_POINT('Ctrl Pts',(104.958734125,4.93750000136559,-1.28537377788739E-14));
#10933=CARTESIAN_POINT('Ctrl Pts',(104.958734125,4.87500000136559,43.4753311640868));
#10934=CARTESIAN_POINT('Ctrl Pts',(74.2170326445434,4.81250000136559,74.2170326445434));
#10935=CARTESIAN_POINT('Ctrl Pts',(43.4753311640869,4.75000000136558,104.958734125));
#10936=CARTESIAN_POINT('Ctrl Pts',(1.92806066683109E-14,4.68750000136558,
104.958734125));
#10937=CARTESIAN_POINT('Ctrl Pts',(-43.4753311640868,4.62500000136559,104.958734125));
#10938=CARTESIAN_POINT('Ctrl Pts',(-74.2170326445434,4.56250000136558,74.2170326445434));
#10939=CARTESIAN_POINT('Ctrl Pts',(-104.958734125,4.50000000136558,43.4753311640869));
#10940=CARTESIAN_POINT('Ctrl Pts',(-104.958734125,4.43750000136558,0.));
#10941=CARTESIAN_POINT('Ctrl Pts',(-104.958734125,4.37500000136558,-43.4753311640868));
#10942=CARTESIAN_POINT('Ctrl Pts',(-74.2170326445434,4.31250000136558,-74.2170326445434));
#10943=CARTESIAN_POINT('Ctrl Pts',(-43.4753311640868,4.25000000136558,-104.958734125));
#10944=CARTESIAN_POINT('Ctrl Pts',(-6.42686888943697E-15,4.18750000136558,
-104.958734125));
#10945=CARTESIAN_POINT('Ctrl Pts',(43.4753311640868,4.12500000136558,-104.958734125));
#10946=CARTESIAN_POINT('Ctrl Pts',(74.2170326445434,4.06250000136558,-74.2170326445434));
#10947=CARTESIAN_POINT('Ctrl Pts',(104.958734125,4.00000000136558,-43.4753311640868));
#10948=CARTESIAN_POINT('Ctrl Pts',(104.958734125,3.93750000136558,-1.28537377788739E-14));
#10949=CARTESIAN_POINT('Ctrl Pts',(104.958734125,3.87500000136558,43.4753311640868));
#10950=CARTESIAN_POINT('Ctrl Pts',(74.2170326445434,3.81250000136558,74.2170326445434));
#10951=CARTESIAN_POINT('Ctrl Pts',(43.4753311640869,3.75000000136558,104.958734125));
#10952=CARTESIAN_POINT('Ctrl Pts',(1.92806066683109E-14,3.68750000136558,
104.958734125));
#10953=CARTESIAN_POINT('Ctrl Pts',(-43.4753311640868,3.62500000136558,104.958734125));
#10954=CARTESIAN_POINT('Ctrl Pts',(-74.2170326445434,3.56250000136558,74.2170326445434));
#10955=CARTESIAN_POINT('Ctrl Pts',(-104.958734125,3.50000000136558,43.4753311640869));
#10956=CARTESIAN_POINT('Ctrl Pts',(-104.958734125,3.43750000136558,0.));
#10957=CARTESIAN_POINT('Ctrl Pts',(-104.958734125,3.37500000136558,-43.4753311640868));
#10958=CARTESIAN_POINT('Ctrl Pts',(-74.2170326445434,3.31250000136558,-74.2170326445434));
#10959=CARTESIAN_POINT('Ctrl Pts',(-43.4753311640868,3.25000000136558,-104.958734125));
#10960=CARTESIAN_POINT('Ctrl Pts',(-6.42686888943697E-15,3.18750000136558,
-104.958734125));
#10961=CARTESIAN_POINT('Ctrl Pts',(43.4753311640868,3.12500000136558,-104.958734125));
#10962=CARTESIAN_POINT('Ctrl Pts',(74.2170326445434,3.06250000136558,-74.2170326445434));
#10963=CARTESIAN_POINT('Ctrl Pts',(104.958734125,3.00000000136558,-43.4753311640868));
#10964=CARTESIAN_POINT('Ctrl Pts',(104.958734125,2.93750000136558,-1.28537377788739E-14));
#10965=CARTESIAN_POINT('Ctrl Pts',(104.958734125,2.87500000136558,43.4753311640868));
#10966=CARTESIAN_POINT('Ctrl Pts',(74.2170326445434,2.81250000136558,74.2170326445434));
#10967=CARTESIAN_POINT('Ctrl Pts',(43.4753311640869,2.75000000136558,104.958734125));
#10968=CARTESIAN_POINT('Ctrl Pts',(1.92806066683109E-14,2.68750000136558,
104.958734125));
#10969=CARTESIAN_POINT('Ctrl Pts',(-43.4753311640868,2.62500000136558,104.958734125));
#10970=CARTESIAN_POINT('Ctrl Pts',(-74.2170326445434,2.56250000136558,74.2170326445434));
#10971=CARTESIAN_POINT('Ctrl Pts',(-104.958734125,2.50000000136558,43.4753311640869));
#10972=CARTESIAN_POINT('Ctrl Pts',(-104.958734125,2.43750000136558,0.));
#10973=CARTESIAN_POINT('Ctrl Pts',(-104.958734125,2.37500000136558,-43.4753311640868));
#10974=CARTESIAN_POINT('Ctrl Pts',(-74.2170326445434,2.31250000136558,-74.2170326445434));
#10975=CARTESIAN_POINT('Ctrl Pts',(-43.4753311640868,2.25000000136558,-104.958734125));
#10976=CARTESIAN_POINT('Ctrl Pts',(-6.42686888943697E-15,2.18750000136558,
-104.958734125));
#10977=CARTESIAN_POINT('Ctrl Pts',(43.4753311640868,2.12500000136558,-104.958734125));
#10978=CARTESIAN_POINT('Ctrl Pts',(74.2170326445434,2.06250000136558,-74.2170326445434));
#10979=CARTESIAN_POINT('Ctrl Pts',(104.958734125,2.00000000136558,-43.4753311640868));
#10980=CARTESIAN_POINT('Ctrl Pts',(104.958734125,1.93750000136558,-1.28537377788739E-14));
#10981=CARTESIAN_POINT('Ctrl Pts',(104.958734125,1.87500000136558,43.4753311640868));
#10982=CARTESIAN_POINT('Ctrl Pts',(74.2170326445434,1.81250000136558,74.2170326445434));
#10983=CARTESIAN_POINT('Ctrl Pts',(43.4753311640869,1.75000000136558,104.958734125));
#10984=CARTESIAN_POINT('Ctrl Pts',(1.92806066683109E-14,1.68750000136558,
104.958734125));
#10985=CARTESIAN_POINT('Ctrl Pts',(-43.4753311640868,1.62500000136558,104.958734125));
#10986=CARTESIAN_POINT('Ctrl Pts',(-74.2170326445434,1.56250000136558,74.2170326445434));
#10987=CARTESIAN_POINT('Ctrl Pts',(-104.958734125,1.50000000136558,43.4753311640869));
#10988=CARTESIAN_POINT('Ctrl Pts',(-104.958734125,1.43750000136558,0.));
#10989=CARTESIAN_POINT('Ctrl Pts',(-104.958734125,1.37500000136558,-43.4753311640868));
#10990=CARTESIAN_POINT('Ctrl Pts',(-74.2170326445434,1.31250000136558,-74.2170326445434));
#10991=CARTESIAN_POINT('Ctrl Pts',(-43.4753311640868,1.25000000136558,-104.958734125));
#10992=CARTESIAN_POINT('Ctrl Pts',(-6.42686888943697E-15,1.18750000136558,
-104.958734125));
#10993=CARTESIAN_POINT('Ctrl Pts',(43.4753311640868,1.12500000136558,-104.958734125));
#10994=CARTESIAN_POINT('Ctrl Pts',(74.2170326445434,1.06250000136558,-74.2170326445434));
#10995=CARTESIAN_POINT('Ctrl Pts',(104.958734125,1.00000000136558,-43.4753311640868));
#10996=CARTESIAN_POINT('Ctrl Pts',(104.958734125,0.937500001365582,-1.28537377788739E-14));
#10997=CARTESIAN_POINT('Ctrl Pts',(104.958734125,0.875000001365582,43.4753311640868));
#10998=CARTESIAN_POINT('Ctrl Pts',(74.2170326445434,0.812500001365582,74.2170326445434));
#10999=CARTESIAN_POINT('Ctrl Pts',(43.4753311640869,0.750000001365582,104.958734125));
#11000=CARTESIAN_POINT('Ctrl Pts',(1.92806066683109E-14,0.687500001365582,
104.958734125));
#11001=CARTESIAN_POINT('Ctrl Pts',(-43.4753311640868,0.625000001365582,
104.958734125));
#11002=CARTESIAN_POINT('Ctrl Pts',(-74.2170326445434,0.562500001365582,
74.2170326445434));
#11003=CARTESIAN_POINT('Ctrl Pts',(-104.958734125,0.500000001365582,43.4753311640869));
#11004=CARTESIAN_POINT('Ctrl Pts',(-104.958734125,0.437500001365582,0.));
#11005=CARTESIAN_POINT('Ctrl Pts',(-104.958734125,0.375000001365582,-43.4753311640868));
#11006=CARTESIAN_POINT('Ctrl Pts',(-74.2170326445434,0.312500001365582,
-74.2170326445434));
#11007=CARTESIAN_POINT('Ctrl Pts',(-43.4753311640868,0.250000001365581,
-104.958734125));
#11008=CARTESIAN_POINT('Ctrl Pts',(-6.42686888943697E-15,0.187500001365581,
-104.958734125));
#11009=CARTESIAN_POINT('Ctrl Pts',(43.4753311640868,0.125000001365581,-104.958734125));
#11010=CARTESIAN_POINT('Ctrl Pts',(74.2170326445434,0.0625000013655813,
-74.2170326445434));
#11011=CARTESIAN_POINT('Ctrl Pts',(104.958734125,1.36558125918285E-9,-43.4753311640868));
#11012=CARTESIAN_POINT('Ctrl Pts',(104.958734125,-0.0624999986344188,-1.28537377788739E-14));
#11013=CARTESIAN_POINT('Ctrl Pts',(104.958734125,-0.124999998634419,43.4753311640868));
#11014=CARTESIAN_POINT('Ctrl Pts',(74.2170326445434,-0.187499998634419,
74.2170326445434));
#11015=CARTESIAN_POINT('Ctrl Pts',(43.4753311640869,-0.249999998634419,
104.958734125));
#11016=CARTESIAN_POINT('Ctrl Pts',(1.92806066683109E-14,-0.312499998634419,
104.958734125));
#11017=CARTESIAN_POINT('Ctrl Pts',(-43.4753311640868,-0.374999998634419,
104.958734125));
#11018=CARTESIAN_POINT('Ctrl Pts',(-74.2170326445434,-0.437499998634419,
74.2170326445434));
#11019=CARTESIAN_POINT('Ctrl Pts',(-104.958734125,-0.499999998634419,43.4753311640869));
#11020=CARTESIAN_POINT('Ctrl Pts',(-104.958734125,-0.562499998634419,0.));
#11021=CARTESIAN_POINT('Ctrl Pts',(-74.5997640648779,1.9358265601193E-15,
-74.5997667654837));
#11022=CARTESIAN_POINT('Ctrl Pts',(-43.6995308303615,-0.0624999972688237,
-105.5));
#11023=CARTESIAN_POINT('Ctrl Pts',(-6.46001186550229E-15,-0.124999997268824,
-105.5));
#11024=CARTESIAN_POINT('Ctrl Pts',(43.6995308303615,-0.187499997268824,
-105.5));
#11025=CARTESIAN_POINT('Ctrl Pts',(74.5997654151808,-0.249999997268824,
-74.5997654151808));
#11026=CARTESIAN_POINT('Ctrl Pts',(105.5,-0.312499997268824,-43.6995308303616));
#11027=CARTESIAN_POINT('Ctrl Pts',(105.5,-0.374999997268824,-1.29200237310046E-14));
#11028=CARTESIAN_POINT('Ctrl Pts',(105.5,-0.437499997268824,43.6995308303615));
#11029=CARTESIAN_POINT('Ctrl Pts',(74.5997654151808,-0.499999997268824,
74.5997654151808));
#11030=CARTESIAN_POINT('Ctrl Pts',(43.6995308303616,-0.562499997268824,
105.5));
#11031=CARTESIAN_POINT('Ctrl Pts',(1.93800355965069E-14,-0.624999997268824,
105.5));
#11032=CARTESIAN_POINT('Ctrl Pts',(-43.6995308303616,-0.687499997268824,
105.5));
#11033=CARTESIAN_POINT('Ctrl Pts',(-74.5997654151808,-0.749999997268824,
74.5997654151808));
#11034=CARTESIAN_POINT('Ctrl Pts',(-105.5,-0.812499997268824,43.6995308303616));
#11035=CARTESIAN_POINT('Ctrl Pts',(-105.5,-0.874999997268824,0.));
#11036=CARTESIAN_POINT('Origin',(0.,105.,0.));
#11037=CARTESIAN_POINT('Origin',(0.,50.,0.));
#11038=CARTESIAN_POINT('',(115.,50.,-9.99999999999999));
#11039=CARTESIAN_POINT('',(0.,50.,-9.99999999999999));
#11040=CARTESIAN_POINT('Origin',(115.,50.,0.));
#11041=CARTESIAN_POINT('Origin',(115.,50.,0.));
#11042=CARTESIAN_POINT('Origin',(0.,50.,0.));
#11043=CARTESIAN_POINT('',(-115.,50.,-9.99999999999999));
#11044=CARTESIAN_POINT('',(0.,50.,-9.99999999999999));
#11045=CARTESIAN_POINT('Origin',(-115.,50.,0.));
#11046=CARTESIAN_POINT('Origin',(-115.,50.,0.));
#11047=CARTESIAN_POINT('Origin',(0.,100.,0.));
#11048=CARTESIAN_POINT('',(-1.4058614088468E-14,100.,-114.797295826488));
#11049=CARTESIAN_POINT('Origin',(0.,10.0000000000002,0.));
#11050=CARTESIAN_POINT('',(-1.47569939297256E-14,10.0000000000002,-120.5));
#11051=CARTESIAN_POINT('',(0.,0.,0.));
#11052=CARTESIAN_POINT('Origin',(215.,50.,0.));
#11053=CARTESIAN_POINT('',(215.,50.,-12.));
#11054=CARTESIAN_POINT('Origin',(215.,50.,0.));
#11055=CARTESIAN_POINT('Origin',(-266.943789971923,50.,0.));
#11056=CARTESIAN_POINT('',(145.,50.,-15.));
#11057=CARTESIAN_POINT('Origin',(145.,50.,0.));
#11058=CARTESIAN_POINT('',(212.,50.,-15.));
#11059=CARTESIAN_POINT('',(-266.943789971923,50.,-15.));
#11060=CARTESIAN_POINT('Origin',(212.,50.,0.));
#11061=CARTESIAN_POINT('Origin',(145.,50.,-15.));
#11062=CARTESIAN_POINT('',(145.,50.,-9.99999999999999));
#11063=CARTESIAN_POINT('Origin',(145.,50.,0.));
#11064=CARTESIAN_POINT('Origin',(-266.943789971923,50.,0.));
#11065=CARTESIAN_POINT('',(115.,50.,-9.99999999999999));
#11066=CARTESIAN_POINT('Origin',(115.,50.,0.));
#11067=CARTESIAN_POINT('',(-266.943789971923,50.,-9.99999999999999));
#11068=CARTESIAN_POINT('Origin',(115.,50.,-9.99999999999998));
#11069=CARTESIAN_POINT('Origin',(212.,50.,0.));
#11070=CARTESIAN_POINT('',(212.,50.,-15.));
#11071=CARTESIAN_POINT('',(0.,0.,0.));
#11072=CARTESIAN_POINT('',(0.,0.0300731601977916,-1.73390069635334));
#11073=CARTESIAN_POINT('',(0.,32.521531146335,46.8455240821518));
#11074=CARTESIAN_POINT('',(0.,0.,0.));
#11075=CARTESIAN_POINT('Origin',(-6.07016839548973E-14,-537.001,260.5));
#11076=CARTESIAN_POINT('',(-12.5,6.3047601064593,260.5));
#11077=CARTESIAN_POINT('',(12.5,6.30476010645914,260.5));
#11078=CARTESIAN_POINT('Ctrl Pts',(-12.5,6.30476010645931,260.5));
#11079=CARTESIAN_POINT('Ctrl Pts',(-12.5,6.30476010645931,261.402519215477));
#11080=CARTESIAN_POINT('Ctrl Pts',(-12.4043127929448,6.50044843544715,262.252785687934));
#11081=CARTESIAN_POINT('Ctrl Pts',(-12.0635561086719,7.11290498732527,263.87784696441));
#11082=CARTESIAN_POINT('Ctrl Pts',(-11.8174017497439,7.5270600588976,264.653397811714));
#11083=CARTESIAN_POINT('Ctrl Pts',(-11.1849437511818,8.43828057198777,266.139053437606));
#11084=CARTESIAN_POINT('Ctrl Pts',(-10.798286104564,8.93532092407379,266.84711374057));
#11085=CARTESIAN_POINT('Ctrl Pts',(-9.90196102753225,9.91938057635149,268.170723777041));
#11086=CARTESIAN_POINT('Ctrl Pts',(-9.39191602949771,10.4067552745245,268.785753500166));
#11087=CARTESIAN_POINT('Ctrl Pts',(-7.80732266462415,11.6967917658663,270.370346865039));
#11088=CARTESIAN_POINT('Ctrl Pts',(-6.47055303401493,12.5222310217994,271.323893855586));
#11089=CARTESIAN_POINT('Ctrl Pts',(-4.17535648184543,13.3878671232299,272.311438876291));
#11090=CARTESIAN_POINT('Ctrl Pts',(-3.36242380893801,13.6166122026276,272.569314105635));
#11091=CARTESIAN_POINT('Ctrl Pts',(-1.69558088010183,13.9227521430804,272.913671589856));
#11092=CARTESIAN_POINT('Ctrl Pts',(-0.841611848845278,14.,273.));
#11093=CARTESIAN_POINT('Ctrl Pts',(0.841611848845341,14.,273.));
#11094=CARTESIAN_POINT('Ctrl Pts',(1.69558088010189,13.9227521430804,272.913671589856));
#11095=CARTESIAN_POINT('Ctrl Pts',(3.36242380893806,13.6166122026275,272.569314105635));
#11096=CARTESIAN_POINT('Ctrl Pts',(4.17535648184549,13.3878671232299,272.311438876291));
#11097=CARTESIAN_POINT('Ctrl Pts',(6.47055303401499,12.5222310217993,271.323893855586));
#11098=CARTESIAN_POINT('Ctrl Pts',(7.80732266462421,11.6967917658663,270.370346865039));
#11099=CARTESIAN_POINT('Ctrl Pts',(9.39191602949777,10.4067552745245,268.785753500166));
#11100=CARTESIAN_POINT('Ctrl Pts',(9.9019610275323,9.91938057635144,268.170723777041));
#11101=CARTESIAN_POINT('Ctrl Pts',(10.7982861045641,8.93532092407374,266.84711374057));
#11102=CARTESIAN_POINT('Ctrl Pts',(11.1849437511818,8.4382805719877,266.139053437606));
#11103=CARTESIAN_POINT('Ctrl Pts',(11.817401749744,7.5270600588975,264.653397811714));
#11104=CARTESIAN_POINT('Ctrl Pts',(12.063556108672,7.11290498732516,263.87784696441));
#11105=CARTESIAN_POINT('Ctrl Pts',(12.4043127929449,6.50044843544704,262.252785687934));
#11106=CARTESIAN_POINT('Ctrl Pts',(12.5,6.30476010645918,261.402519215477));
#11107=CARTESIAN_POINT('Ctrl Pts',(12.5,6.30476010645918,260.5));
#11108=CARTESIAN_POINT('Ctrl Pts',(12.5,6.30476010645918,260.5));
#11109=CARTESIAN_POINT('Ctrl Pts',(12.5,6.30476010645918,259.597480784523));
#11110=CARTESIAN_POINT('Ctrl Pts',(12.4043127929449,6.50044843544704,258.747214312066));
#11111=CARTESIAN_POINT('Ctrl Pts',(12.063556108672,7.11290498732516,257.12215303559));
#11112=CARTESIAN_POINT('Ctrl Pts',(11.817401749744,7.5270600588975,256.346602188286));
#11113=CARTESIAN_POINT('Ctrl Pts',(11.1849437511818,8.4382805719877,254.860946562394));
#11114=CARTESIAN_POINT('Ctrl Pts',(10.7982861045641,8.93532092407371,254.15288625943));
#11115=CARTESIAN_POINT('Ctrl Pts',(9.90196102753233,9.91938057635141,252.829276222959));
#11116=CARTESIAN_POINT('Ctrl Pts',(9.39191602949779,10.4067552745245,252.214246499834));
#11117=CARTESIAN_POINT('Ctrl Pts',(7.80732266462423,11.6967917658663,250.629653134961));
#11118=CARTESIAN_POINT('Ctrl Pts',(6.47055303401501,12.5222310217993,249.676106144414));
#11119=CARTESIAN_POINT('Ctrl Pts',(4.17535648184551,13.3878671232299,248.688561123709));
#11120=CARTESIAN_POINT('Ctrl Pts',(3.36242380893808,13.6166122026275,248.430685894365));
#11121=CARTESIAN_POINT('Ctrl Pts',(1.6955808801019,13.9227521430804,248.086328410144));
#11122=CARTESIAN_POINT('Ctrl Pts',(0.841611848845347,14.,248.));
#11123=CARTESIAN_POINT('Ctrl Pts',(-0.841611848845273,14.,248.));
#11124=CARTESIAN_POINT('Ctrl Pts',(-1.69558088010183,13.9227521430804,248.086328410144));
#11125=CARTESIAN_POINT('Ctrl Pts',(-3.362423808938,13.6166122026276,248.430685894365));
#11126=CARTESIAN_POINT('Ctrl Pts',(-4.17535648184543,13.3878671232299,248.688561123709));
#11127=CARTESIAN_POINT('Ctrl Pts',(-6.47055303401493,12.5222310217994,249.676106144414));
#11128=CARTESIAN_POINT('Ctrl Pts',(-7.80732266462415,11.6967917658663,250.629653134961));
#11129=CARTESIAN_POINT('Ctrl Pts',(-9.39191602949771,10.4067552745245,252.214246499834));
#11130=CARTESIAN_POINT('Ctrl Pts',(-9.90196102753228,9.91938057635146,252.829276222959));
#11131=CARTESIAN_POINT('Ctrl Pts',(-10.7982861045641,8.93532092407377,254.15288625943));
#11132=CARTESIAN_POINT('Ctrl Pts',(-11.1849437511818,8.43828057198777,254.860946562394));
#11133=CARTESIAN_POINT('Ctrl Pts',(-11.8174017497439,7.5270600588976,256.346602188286));
#11134=CARTESIAN_POINT('Ctrl Pts',(-12.0635561086719,7.11290498732527,257.122153035591));
#11135=CARTESIAN_POINT('Ctrl Pts',(-12.4043127929448,6.50044843544715,258.747214312066));
#11136=CARTESIAN_POINT('Ctrl Pts',(-12.5,6.30476010645931,259.597480784523));
#11137=CARTESIAN_POINT('Ctrl Pts',(-12.5,6.30476010645931,260.5));
#11138=CARTESIAN_POINT('',(12.5,15.,260.5));
#11139=CARTESIAN_POINT('',(12.4999999999999,-537.001,260.5));
#11140=CARTESIAN_POINT('Origin',(3.50552253913701E-14,15.,260.5));
#11141=CARTESIAN_POINT('Origin',(0.,0.,288.5));
#11142=CARTESIAN_POINT('',(15.,-1.83697019872103E-15,288.5));
#11143=CARTESIAN_POINT('Origin',(0.,0.,288.5));
#11144=CARTESIAN_POINT('',(14.,-1.71450551880629E-15,288.5));
#11145=CARTESIAN_POINT('Origin',(0.,0.,288.5));
#11146=CARTESIAN_POINT('Origin',(0.,0.,125.5));
#11147=CARTESIAN_POINT('',(15.,-1.83697019872103E-15,125.5));
#11148=CARTESIAN_POINT('Origin',(0.,0.,125.5));
#11149=CARTESIAN_POINT('',(14.,-1.71450551880629E-15,125.5));
#11150=CARTESIAN_POINT('Origin',(0.,0.,125.5));
#11151=CARTESIAN_POINT('Origin',(0.,0.,288.5));
#11152=CARTESIAN_POINT('',(15.,-1.83697019872103E-15,288.5));
#11153=CARTESIAN_POINT('',(-13.5,6.53834841531107,260.5));
#11154=CARTESIAN_POINT('',(13.5,6.53834841531101,260.5));
#11155=CARTESIAN_POINT('Ctrl Pts',(-13.5,6.53834841531108,260.5));
#11156=CARTESIAN_POINT('Ctrl Pts',(-13.5,6.53834841531108,261.480875587233));
#11157=CARTESIAN_POINT('Ctrl Pts',(-13.3958232026777,6.76037527468857,262.398034825266));
#11158=CARTESIAN_POINT('Ctrl Pts',(-13.0281423324427,7.44434384956079,264.149401104853));
#11159=CARTESIAN_POINT('Ctrl Pts',(-12.7631917195318,7.9038410644566,264.984257909941));
#11160=CARTESIAN_POINT('Ctrl Pts',(-12.0815890679171,8.91094016019654,266.586308189152));
#11161=CARTESIAN_POINT('Ctrl Pts',(-11.6646347002389,9.45851405605539,267.350709749346));
#11162=CARTESIAN_POINT('Ctrl Pts',(-10.6965567278803,10.5409138836385,268.78128013682));
#11163=CARTESIAN_POINT('Ctrl Pts',(-10.1450315382585,11.0761700594821,269.446851553778));
#11164=CARTESIAN_POINT('Ctrl Pts',(-8.43405624607796,12.487773690397,271.157826845959));
#11165=CARTESIAN_POINT('Ctrl Pts',(-6.99182923331508,13.388092684802,272.187651131601));
#11166=CARTESIAN_POINT('Ctrl Pts',(-4.51318011101059,14.332232492506,273.255015840138));
#11167=CARTESIAN_POINT('Ctrl Pts',(-3.63493173087046,14.5817163893703,273.533927767516));
#11168=CARTESIAN_POINT('Ctrl Pts',(-1.83348931439436,14.9156796189506,273.906502850605));
#11169=CARTESIAN_POINT('Ctrl Pts',(-0.910231484953233,15.,274.));
#11170=CARTESIAN_POINT('Ctrl Pts',(0.910231484953305,15.,274.));
#11171=CARTESIAN_POINT('Ctrl Pts',(1.83348931439444,14.9156796189506,273.906502850605));
#11172=CARTESIAN_POINT('Ctrl Pts',(3.63493173087052,14.5817163893703,273.533927767516));
#11173=CARTESIAN_POINT('Ctrl Pts',(4.51318011101065,14.332232492506,273.255015840138));
#11174=CARTESIAN_POINT('Ctrl Pts',(6.99182923331514,13.3880926848019,272.187651131601));
#11175=CARTESIAN_POINT('Ctrl Pts',(8.43405624607803,12.4877736903969,271.157826845959));
#11176=CARTESIAN_POINT('Ctrl Pts',(10.1450315382585,11.0761700594821,269.446851553778));
#11177=CARTESIAN_POINT('Ctrl Pts',(10.6965567278803,10.5409138836385,268.78128013682));
#11178=CARTESIAN_POINT('Ctrl Pts',(11.664634700239,9.45851405605531,267.350709749346));
#11179=CARTESIAN_POINT('Ctrl Pts',(12.0815890679171,8.91094016019645,266.586308189152));
#11180=CARTESIAN_POINT('Ctrl Pts',(12.7631917195319,7.90384106445649,264.984257909941));
#11181=CARTESIAN_POINT('Ctrl Pts',(13.0281423324427,7.44434384956068,264.149401104853));
#11182=CARTESIAN_POINT('Ctrl Pts',(13.3958232026778,6.76037527468845,262.398034825266));
#11183=CARTESIAN_POINT('Ctrl Pts',(13.5,6.53834841531094,261.480875587233));
#11184=CARTESIAN_POINT('Ctrl Pts',(13.5,6.53834841531094,260.5));
#11185=CARTESIAN_POINT('Ctrl Pts',(13.5,6.53834841531094,260.5));
#11186=CARTESIAN_POINT('Ctrl Pts',(13.5,6.53834841531094,259.519124412767));
#11187=CARTESIAN_POINT('Ctrl Pts',(13.3958232026778,6.76037527468844,258.601965174734));
#11188=CARTESIAN_POINT('Ctrl Pts',(13.0281423324427,7.44434384956067,256.850598895147));
#11189=CARTESIAN_POINT('Ctrl Pts',(12.7631917195319,7.90384106445648,256.015742090059));
#11190=CARTESIAN_POINT('Ctrl Pts',(12.0815890679171,8.91094016019645,254.413691810848));
#11191=CARTESIAN_POINT('Ctrl Pts',(11.664634700239,9.4585140560553,253.649290250654));
#11192=CARTESIAN_POINT('Ctrl Pts',(10.6965567278803,10.5409138836385,252.21871986318));
#11193=CARTESIAN_POINT('Ctrl Pts',(10.1450315382585,11.0761700594821,251.553148446222));
#11194=CARTESIAN_POINT('Ctrl Pts',(8.43405624607803,12.4877736903969,249.842173154041));
#11195=CARTESIAN_POINT('Ctrl Pts',(6.99182923331515,13.3880926848019,248.812348868399));
#11196=CARTESIAN_POINT('Ctrl Pts',(4.51318011101067,14.332232492506,247.744984159862));
#11197=CARTESIAN_POINT('Ctrl Pts',(3.63493173087054,14.5817163893703,247.466072232484));
#11198=CARTESIAN_POINT('Ctrl Pts',(1.83348931439444,14.9156796189506,247.093497149395));
#11199=CARTESIAN_POINT('Ctrl Pts',(0.910231484953304,15.,247.));
#11200=CARTESIAN_POINT('Ctrl Pts',(-0.910231484953234,15.,247.));
#11201=CARTESIAN_POINT('Ctrl Pts',(-1.83348931439437,14.9156796189506,247.093497149395));
#11202=CARTESIAN_POINT('Ctrl Pts',(-3.63493173087047,14.5817163893703,247.466072232484));
#11203=CARTESIAN_POINT('Ctrl Pts',(-4.51318011101059,14.332232492506,247.744984159862));
#11204=CARTESIAN_POINT('Ctrl Pts',(-6.99182923331508,13.388092684802,248.812348868399));
#11205=CARTESIAN_POINT('Ctrl Pts',(-8.43405624607796,12.487773690397,249.842173154041));
#11206=CARTESIAN_POINT('Ctrl Pts',(-10.1450315382585,11.0761700594821,251.553148446222));
#11207=CARTESIAN_POINT('Ctrl Pts',(-10.6965567278803,10.5409138836385,252.21871986318));
#11208=CARTESIAN_POINT('Ctrl Pts',(-11.6646347002389,9.45851405605539,253.649290250654));
#11209=CARTESIAN_POINT('Ctrl Pts',(-12.0815890679171,8.91094016019654,254.413691810848));
#11210=CARTESIAN_POINT('Ctrl Pts',(-12.7631917195318,7.9038410644566,256.015742090059));
#11211=CARTESIAN_POINT('Ctrl Pts',(-13.0281423324427,7.44434384956078,256.850598895147));
#11212=CARTESIAN_POINT('Ctrl Pts',(-13.3958232026777,6.76037527468857,258.601965174734));
#11213=CARTESIAN_POINT('Ctrl Pts',(-13.5,6.53834841531108,259.519124412767));
#11214=CARTESIAN_POINT('Ctrl Pts',(-13.5,6.53834841531108,260.5));
#11215=CARTESIAN_POINT('Origin',(0.,0.,288.5));
#11216=CARTESIAN_POINT('',(14.,-1.71450551880629E-15,288.5));
#11217=CARTESIAN_POINT('Origin',(-6.07016839548973E-14,-537.001,260.5));
#11218=CARTESIAN_POINT('',(13.5,20.,260.5));
#11219=CARTESIAN_POINT('Origin',(3.59225871293585E-14,20.,260.5));
#11220=CARTESIAN_POINT('',(13.4999999999999,-537.001,260.5));
#11221=CARTESIAN_POINT('Origin',(3.59225871293585E-14,20.,260.5));
#11222=CARTESIAN_POINT('',(12.5,20.,260.5));
#11223=CARTESIAN_POINT('Origin',(3.59225871293585E-14,20.,260.5));
#11224=CARTESIAN_POINT('Origin',(3.50552253913701E-14,15.,260.5));
#11225=CARTESIAN_POINT('',(12.5,40.,260.5));
#11226=CARTESIAN_POINT('Origin',(3.93920340813121E-14,40.,260.5));
#11227=CARTESIAN_POINT('',(12.5,15.,260.5));
#11228=CARTESIAN_POINT('Origin',(3.50552253913701E-14,15.,260.5));
#11229=CARTESIAN_POINT('',(11.5,15.,260.5));
#11230=CARTESIAN_POINT('Origin',(3.50552253913701E-14,15.,260.5));
#11231=CARTESIAN_POINT('Origin',(3.50552253913701E-14,15.,260.5));
#11232=CARTESIAN_POINT('',(11.5,40.,260.5));
#11233=CARTESIAN_POINT('',(11.5,15.,260.5));
#11234=CARTESIAN_POINT('Origin',(3.93920340813121E-14,40.,260.5));
#11235=CARTESIAN_POINT('Origin',(3.93920340813121E-14,40.,260.5));
#11236=CARTESIAN_POINT('',(0.,0.,0.));
#11237=CARTESIAN_POINT('Origin',(200.,150.,0.));
#11238=CARTESIAN_POINT('',(-2.47378653427765E-14,150.,-202.));
#11239=CARTESIAN_POINT('Origin',(0.,150.,0.));
#11240=CARTESIAN_POINT('',(-2.44929359829471E-14,150.,-200.));
#11241=CARTESIAN_POINT('Origin',(0.,150.,0.));
#11242=CARTESIAN_POINT('Origin',(0.,-150.,0.));
#11243=CARTESIAN_POINT('',(0.,-150.,-52.));
#11244=CARTESIAN_POINT('',(-6.36816335556624E-15,-150.,-52.));
#11245=CARTESIAN_POINT('Origin',(0.,-150.,0.));
#11246=CARTESIAN_POINT('Origin',(0.,150.,0.));
#11247=CARTESIAN_POINT('',(-6.12323399573677E-15,-150.,-50.0000000000001));
#11248=CARTESIAN_POINT('Origin',(0.,-150.,0.));
#11249=CARTESIAN_POINT('',(-2.44929359829471E-14,150.,-200.));
#11250=CARTESIAN_POINT('Origin',(0.,-170.,0.));
#11251=CARTESIAN_POINT('',(0.,-170.,-50.));
#11252=CARTESIAN_POINT('Origin',(0.,-170.,0.));
#11253=CARTESIAN_POINT('',(-6.12323399573677E-15,-170.,-50.));
#11254=CARTESIAN_POINT('Origin',(0.,-170.,0.));
#11255=CARTESIAN_POINT('',(0.,-152.,-52.));
#11256=CARTESIAN_POINT('Origin',(0.,-152.,0.));
#11257=CARTESIAN_POINT('',(0.,-170.,-52.));
#11258=CARTESIAN_POINT('',(-6.36816335556624E-15,-170.,-52.));
#11259=CARTESIAN_POINT('Origin',(0.,-170.,0.));
#11260=CARTESIAN_POINT('Origin',(0.,-170.,0.));
#11261=CARTESIAN_POINT('Origin',(0.,-152.,0.));
#11262=CARTESIAN_POINT('',(0.,-150.,-56.));
#11263=CARTESIAN_POINT('Origin',(0.,-150.,0.));
#11264=CARTESIAN_POINT('',(0.,-152.,-56.));
#11265=CARTESIAN_POINT('',(-6.85802207522518E-15,-152.,-56.));
#11266=CARTESIAN_POINT('Origin',(0.,-152.,0.));
#11267=CARTESIAN_POINT('Origin',(0.,-152.,0.));
#11268=CARTESIAN_POINT('Origin',(0.,-150.,0.));
#11269=CARTESIAN_POINT('',(0.,0.,0.));
#11270=CARTESIAN_POINT('Origin',(4.28614810332657E-14,460.,100.5));
#11271=CARTESIAN_POINT('',(4.10245108345447E-14,460.,115.5));
#11272=CARTESIAN_POINT('Origin',(4.28614810332657E-14,460.,100.5));
#11273=CARTESIAN_POINT('',(4.11469755144594E-14,460.,114.5));
#11274=CARTESIAN_POINT('Origin',(4.28614810332657E-14,460.,100.5));
#11275=CARTESIAN_POINT('Origin',(4.28614810332657E-14,460.,180.5));
#11276=CARTESIAN_POINT('',(4.10245108345447E-14,460.,245.5));
#11277=CARTESIAN_POINT('',(4.10245108345447E-14,460.,275.5));
#11278=CARTESIAN_POINT('Origin',(4.28614810332657E-14,460.,260.5));
#11279=CARTESIAN_POINT('Origin',(4.28614810332657E-14,460.,260.5));
#11280=CARTESIAN_POINT('Origin',(4.10245108345447E-14,460.,180.5));
#11281=CARTESIAN_POINT('Origin',(4.28614810332657E-14,460.,260.5));
#11282=CARTESIAN_POINT('',(4.10245108345447E-14,57.,275.5));
#11283=CARTESIAN_POINT('Origin',(4.23410639904727E-14,57.,260.5));
#11284=CARTESIAN_POINT('',(4.10245108345447E-14,460.,275.5));
#11285=CARTESIAN_POINT('Origin',(4.28614810332657E-14,460.,180.5));
#11286=CARTESIAN_POINT('',(4.11469755144594E-14,460.,246.5));
#11287=CARTESIAN_POINT('Origin',(4.11469755144594E-14,460.,180.5));
#11288=CARTESIAN_POINT('',(4.28614810332657E-14,460.,274.5));
#11289=CARTESIAN_POINT('Origin',(4.28614810332657E-14,460.,260.5));
#11290=CARTESIAN_POINT('Origin',(4.28614810332657E-14,460.,260.5));
#11291=CARTESIAN_POINT('Origin',(4.28614810332657E-14,460.,260.5));
#11292=CARTESIAN_POINT('',(4.11469755144594E-14,60.,274.5));
#11293=CARTESIAN_POINT('',(4.11469755144594E-14,460.,274.5));
#11294=CARTESIAN_POINT('Origin',(4.28614810332657E-14,60.,260.5));
#11295=CARTESIAN_POINT('Origin',(4.28614810332657E-14,60.,260.5));
#11296=CARTESIAN_POINT('',(11.,60.,260.5));
#11297=CARTESIAN_POINT('Origin',(4.28614810332657E-14,60.,260.5));
#11298=CARTESIAN_POINT('Origin',(4.28614810332657E-14,60.,260.5));
#11299=CARTESIAN_POINT('',(-12.5,50.,260.5));
#11300=CARTESIAN_POINT('Origin',(4.11267575572889E-14,50.,260.5));
#11301=CARTESIAN_POINT('',(-12.5,57.,260.5));
#11302=CARTESIAN_POINT('',(-12.5,60.,260.5));
#11303=CARTESIAN_POINT('Origin',(4.23410639904727E-14,57.,260.5));
#11304=CARTESIAN_POINT('Origin',(4.28614810332657E-14,60.,260.5));
#11305=CARTESIAN_POINT('',(-11.5,57.,260.5));
#11306=CARTESIAN_POINT('Origin',(4.23410639904727E-14,57.,260.5));
#11307=CARTESIAN_POINT('',(-11.5,50.,260.5));
#11308=CARTESIAN_POINT('',(-11.5,60.,260.5));
#11309=CARTESIAN_POINT('Origin',(4.11267575572889E-14,50.,260.5));
#11310=CARTESIAN_POINT('Origin',(4.11267575572889E-14,50.,260.5));
#11311=CARTESIAN_POINT('Origin',(4.23410639904727E-14,57.,260.5));
#11312=CARTESIAN_POINT('',(11.,57.,260.5));
#11313=CARTESIAN_POINT('Origin',(4.23410639904727E-14,57.,260.5));
#11314=CARTESIAN_POINT('Origin',(4.23410639904727E-14,57.,260.5));
#11315=CARTESIAN_POINT('',(11.,57.,260.5));
#11316=CARTESIAN_POINT('Origin',(4.23410639904727E-14,57.,260.5));
#11317=CARTESIAN_POINT('',(0.,0.,0.));
#11318=CARTESIAN_POINT('Origin',(0.,240.,0.));
#11319=CARTESIAN_POINT('',(-1.90241102001116E-16,217.99585953923,7.50000000439337));
#11320=CARTESIAN_POINT('',(-4.06843950140785E-7,234.921557632927,7.50242802810186));
#11321=CARTESIAN_POINT('',(-9.18485099360515E-16,240.,7.5));
#11322=CARTESIAN_POINT('',(-9.18479639923619E-16,237.99585953923,7.50000000439337));
#11323=CARTESIAN_POINT('Ctrl Pts',(-9.1847417994869E-16,237.99585953923,
7.50000000439337));
#11324=CARTESIAN_POINT('Ctrl Pts',(-1.18775172812193,237.495912211348,7.50000000439337));
#11325=CARTESIAN_POINT('Ctrl Pts',(-2.317383311169,236.995967593475,7.13300320026677));
#11326=CARTESIAN_POINT('Ctrl Pts',(-3.44714003087638,236.495967593475,6.76596574150984));
#11327=CARTESIAN_POINT('Ctrl Pts',(-4.40818170865423,235.995967593475,6.06777834873578));
#11328=CARTESIAN_POINT('Ctrl Pts',(-5.36922338643209,235.495967593475,5.36959095596173));
#11329=CARTESIAN_POINT('Ctrl Pts',(-6.06747656688843,234.995967593475,4.40859707573286));
#11330=CARTESIAN_POINT('Ctrl Pts',(-6.76572974734476,234.495967593475,3.447603195504));
#11331=CARTESIAN_POINT('Ctrl Pts',(-7.13284454416054,233.995967593475,2.31787160445521));
#11332=CARTESIAN_POINT('Ctrl Pts',(-7.49995934097631,233.495967593475,1.18814001340642));
#11333=CARTESIAN_POINT('Ctrl Pts',(-7.5,232.995967593475,0.000256710972401669));
#11334=CARTESIAN_POINT('Ctrl Pts',(-7.50004065902369,232.495967593475,-1.18762659146162));
#11335=CARTESIAN_POINT('Ctrl Pts',(-7.13300320026677,231.995967593475,-2.317383311169));
#11336=CARTESIAN_POINT('Ctrl Pts',(-6.76596574150984,231.495967593475,-3.44714003087638));
#11337=CARTESIAN_POINT('Ctrl Pts',(-6.06777834873578,230.995967593475,-4.40818170865423));
#11338=CARTESIAN_POINT('Ctrl Pts',(-5.36959095596173,230.495967593475,-5.36922338643209));
#11339=CARTESIAN_POINT('Ctrl Pts',(-4.40859707573286,229.995967593475,-6.06747656688843));
#11340=CARTESIAN_POINT('Ctrl Pts',(-3.447603195504,229.495967593475,-6.76572974734476));
#11341=CARTESIAN_POINT('Ctrl Pts',(-2.31787160445521,228.995967593475,-7.13284454416054));
#11342=CARTESIAN_POINT('Ctrl Pts',(-1.18814001340642,228.495967593475,-7.49995934097631));
#11343=CARTESIAN_POINT('Ctrl Pts',(-0.000256710972402128,227.995967593475,
-7.5));
#11344=CARTESIAN_POINT('Ctrl Pts',(1.18762659146162,227.495967593475,-7.50004065902369));
#11345=CARTESIAN_POINT('Ctrl Pts',(2.317383311169,226.995967593475,-7.13300320026677));
#11346=CARTESIAN_POINT('Ctrl Pts',(3.44714003087638,226.495967593475,-6.76596574150984));
#11347=CARTESIAN_POINT('Ctrl Pts',(4.40818170865423,225.995967593475,-6.06777834873578));
#11348=CARTESIAN_POINT('Ctrl Pts',(5.36922338643209,225.495967593475,-5.36959095596173));
#11349=CARTESIAN_POINT('Ctrl Pts',(6.06747656688843,224.995967593475,-4.40859707573286));
#11350=CARTESIAN_POINT('Ctrl Pts',(6.76572974734476,224.495967593475,-3.447603195504));
#11351=CARTESIAN_POINT('Ctrl Pts',(7.13284454416054,223.995967593475,-2.31787160445521));
#11352=CARTESIAN_POINT('Ctrl Pts',(7.49995934097631,223.495967593475,-1.18814001340642));
#11353=CARTESIAN_POINT('Ctrl Pts',(7.5,222.995967593475,-0.000256710972402588));
#11354=CARTESIAN_POINT('Ctrl Pts',(7.50004065902369,222.495967593475,1.18762659146162));
#11355=CARTESIAN_POINT('Ctrl Pts',(7.13300320026677,221.995967593475,2.317383311169));
#11356=CARTESIAN_POINT('Ctrl Pts',(6.76596574150984,221.495967593475,3.44714003087638));
#11357=CARTESIAN_POINT('Ctrl Pts',(6.06777834873579,220.995967593475,4.40818170865423));
#11358=CARTESIAN_POINT('Ctrl Pts',(5.36959095596173,220.495967593475,5.36922338643209));
#11359=CARTESIAN_POINT('Ctrl Pts',(4.40859707573286,219.995967593475,6.06747656688843));
#11360=CARTESIAN_POINT('Ctrl Pts',(3.447603195504,219.495967593475,6.76572974734476));
#11361=CARTESIAN_POINT('Ctrl Pts',(2.31787160445521,218.995967593475,7.13284454416054));
#11362=CARTESIAN_POINT('Ctrl Pts',(1.18814001340643,218.495967593475,7.49995934097631));
#11363=CARTESIAN_POINT('Ctrl Pts',(0.00025671097240121,217.995967593475,
7.5));
#11364=CARTESIAN_POINT('Ctrl Pts',(0.000128355486249734,217.995913566499,
7.50000000439337));
#11365=CARTESIAN_POINT('Ctrl Pts',(5.38002895896315E-16,217.99585953923,
7.50000000439337));
#11366=CARTESIAN_POINT('',(0.,240.,7.5));
#11367=CARTESIAN_POINT('',(-9.18485099360515E-16,240.,7.5));
#11368=CARTESIAN_POINT('Origin',(0.,240.,0.));
#11369=CARTESIAN_POINT('',(0.00025671099249169,237.995967593476,7.49999999788428));
#11370=CARTESIAN_POINT('Ctrl Pts',(0.00025671097240121,237.995967593475,
7.5));
#11371=CARTESIAN_POINT('Ctrl Pts',(0.000128355486236195,237.995913566499,
7.50000000439337));
#11372=CARTESIAN_POINT('Ctrl Pts',(-9.1847417994869E-16,237.99585953923,
7.50000000439337));
#11373=CARTESIAN_POINT('',(0.19085679599498,235.002028447937,7.49999995822451));
#11374=CARTESIAN_POINT('Origin',(-5.20522648770767E-6,238.000081810591,
-1851.55088195117));
#11375=CARTESIAN_POINT('Ctrl Pts',(0.190856796705285,235.002028447915,7.5));
#11376=CARTESIAN_POINT('Ctrl Pts',(0.127311648028415,234.975281229334,7.50161706980302));
#11377=CARTESIAN_POINT('Ctrl Pts',(0.0636823578853783,234.948453397593,
7.50242803155527));
#11378=CARTESIAN_POINT('Ctrl Pts',(-4.06843934450864E-7,234.921557632927,
7.50242802810186));
#11379=CARTESIAN_POINT('Origin',(0.,240.,0.));
#11380=CARTESIAN_POINT('',(0.,150.,7.5));
#11381=CARTESIAN_POINT('Origin',(0.,150.,0.));
#11382=CARTESIAN_POINT('',(-4.0684396522591E-7,194.921557632927,7.50242802810186));
#11383=CARTESIAN_POINT('',(-9.18485099360515E-16,240.,7.5));
#11384=CARTESIAN_POINT('',(0.190870214476193,175.002034095778,7.4999996458277));
#11385=CARTESIAN_POINT('Ctrl Pts',(-4.06843965232862E-7,194.921557632927,
7.50242802810186));
#11386=CARTESIAN_POINT('Ctrl Pts',(-0.152090385415712,194.857323985265,
7.50242801985428));
#11387=CARTESIAN_POINT('Ctrl Pts',(-0.304485788637936,194.792702491972,
7.49779895914529));
#11388=CARTESIAN_POINT('Ctrl Pts',(-0.456762644214526,194.727870534021,
7.48851081348613));
#11389=CARTESIAN_POINT('Ctrl Pts',(-0.609070650330248,194.663025313709,
7.47922076779598));
#11390=CARTESIAN_POINT('Ctrl Pts',(-0.761259533137463,194.597969762789,
7.46526968655078));
#11391=CARTESIAN_POINT('Ctrl Pts',(-0.91290272043789,194.532885263598,7.44667945730617));
#11392=CARTESIAN_POINT('Ctrl Pts',(-1.06450493068591,194.467818351553,7.42809425151703));
#11393=CARTESIAN_POINT('Ctrl Pts',(-1.2155612127976,194.402722732839,7.40487246128588));
#11394=CARTESIAN_POINT('Ctrl Pts',(-1.36565093134532,194.337780178401,7.37708776215684));
#11395=CARTESIAN_POINT('Ctrl Pts',(-1.51579830432436,194.272812677376,7.34929239000474));
#11396=CARTESIAN_POINT('Ctrl Pts',(-1.6649778616245,194.207998581557,7.31693074896081));
#11397=CARTESIAN_POINT('Ctrl Pts',(-1.81278187771196,194.143517028959,7.28012693438018));
#11398=CARTESIAN_POINT('Ctrl Pts',(-1.92135204017681,194.096151789321,7.25309251248746));
#11399=CARTESIAN_POINT('Ctrl Pts',(-2.02918025203168,194.04896593395,7.22366229239575));
#11400=CARTESIAN_POINT('Ctrl Pts',(-2.13611185762632,194.002028447915,7.19190186588755));
#11401=CARTESIAN_POINT('Ctrl Pts',(-2.2816613117044,193.938139708658,7.14867131011455));
#11402=CARTESIAN_POINT('Ctrl Pts',(-2.42624566734731,193.87379055128,7.10091475754277));
#11403=CARTESIAN_POINT('Ctrl Pts',(-2.56944875671864,193.809155844927,7.04871331545309));
#11404=CARTESIAN_POINT('Ctrl Pts',(-2.71813540129491,193.74204613624,6.99451296753858));
#11405=CARTESIAN_POINT('Ctrl Pts',(-2.86533230206808,193.674628800623,6.93552054364116));
#11406=CARTESIAN_POINT('Ctrl Pts',(-3.01058579312346,193.607105531561,6.87188471229631));
#11407=CARTESIAN_POINT('Ctrl Pts',(-3.15046347852857,193.542081286575,6.81060403165537));
#11408=CARTESIAN_POINT('Ctrl Pts',(-3.28853853492898,193.476959054234,6.74501779444794));
#11409=CARTESIAN_POINT('Ctrl Pts',(-3.42442461876489,193.411920847683,6.67530840839924));
#11410=CARTESIAN_POINT('Ctrl Pts',(-3.5602870648691,193.346893954694,6.60561114847646));
#11411=CARTESIAN_POINT('Ctrl Pts',(-3.693960843474,193.281951283189,6.53179244342482));
#11412=CARTESIAN_POINT('Ctrl Pts',(-3.82508551083643,193.217273190526,6.45407988420021));
#11413=CARTESIAN_POINT('Ctrl Pts',(-3.95624536474471,193.152577741872,6.37634647125995));
#11414=CARTESIAN_POINT('Ctrl Pts',(-4.0848543388159,193.088147231022,6.2947174573996));
#11415=CARTESIAN_POINT('Ctrl Pts',(-4.21058385833655,193.024157275819,6.20946132033724));
#11416=CARTESIAN_POINT('Ctrl Pts',(-4.22508868089454,193.016775056041,6.1996257213086));
#11417=CARTESIAN_POINT('Ctrl Pts',(-4.23955521930311,193.009398692253,6.18974188939153));
#11418=CARTESIAN_POINT('Ctrl Pts',(-4.25398300016701,193.002028447915,6.17981026821526));
#11419=CARTESIAN_POINT('Ctrl Pts',(-4.37904978050105,192.938139708658,6.09371831161215));
#11420=CARTESIAN_POINT('Ctrl Pts',(-4.50180008775214,192.87379055128,6.00362010807856));
#11421=CARTESIAN_POINT('Ctrl Pts',(-4.62186318631576,192.809155844927,5.90972139815641));
#11422=CARTESIAN_POINT('Ctrl Pts',(-4.74652375991947,192.74204613624,5.8122271040762));
#11423=CARTESIAN_POINT('Ctrl Pts',(-4.86828667005456,192.674628800622,5.71063563105828));
#11424=CARTESIAN_POINT('Ctrl Pts',(-4.98676639590067,192.607105531561,5.6052285617595));
#11425=CARTESIAN_POINT('Ctrl Pts',(-5.10086120834454,192.542081286575,5.50372258918893));
#11426=CARTESIAN_POINT('Ctrl Pts',(-5.21191112857775,192.476959054234,5.39867883198654));
#11427=CARTESIAN_POINT('Ctrl Pts',(-5.31960508912721,192.411920847683,5.29039015693365));
#11428=CARTESIAN_POINT('Ctrl Pts',(-5.42728031603782,192.346893954693,5.18212031897172));
#11429=CARTESIAN_POINT('Ctrl Pts',(-5.53160039987492,192.281951283188,5.07060708921572));
#11430=CARTESIAN_POINT('Ctrl Pts',(-5.632292867741,192.217273190525,4.95617830276943));
#11431=CARTESIAN_POINT('Ctrl Pts',(-5.73301235584602,192.152577741871,4.84171881002288));
#11432=CARTESIAN_POINT('Ctrl Pts',(-5.83010200617219,192.088147231023,4.72434264585674));
#11433=CARTESIAN_POINT('Ctrl Pts',(-5.92333228977468,192.02415727582,4.60440668292466));
#11434=CARTESIAN_POINT('Ctrl Pts',(-5.93408782853699,192.016775056042,4.59057023570531));
#11435=CARTESIAN_POINT('Ctrl Pts',(-5.94479205212731,192.009398692253,4.5766997467359));
#11436=CARTESIAN_POINT('Ctrl Pts',(-5.95544464740897,192.002028447915,4.56279578422008));
#11437=CARTESIAN_POINT('Ctrl Pts',(-6.04778634614874,191.938139708657,4.44226970733661));
#11438=CARTESIAN_POINT('Ctrl Pts',(-6.13668694968295,191.87379055128,4.31864929275364));
#11439=CARTESIAN_POINT('Ctrl Pts',(-6.22185744482296,191.809155844926,4.19224477495645));
#11440=CARTESIAN_POINT('Ctrl Pts',(-6.31028930194836,191.742046136239,4.0609999554979));
#11441=CARTESIAN_POINT('Ctrl Pts',(-6.39469921942917,191.674628800622,3.92675391456802));
#11442=CARTESIAN_POINT('Ctrl Pts',(-6.47480755900329,191.60710553156,3.78989358567263));
#11443=CARTESIAN_POINT('Ctrl Pts',(-6.55195110329862,191.542081286575,3.65809843300132));
#11444=CARTESIAN_POINT('Ctrl Pts',(-6.6251055474419,191.476959054234,3.5238795706418));
#11445=CARTESIAN_POINT('Ctrl Pts',(-6.69406554949839,191.411920847682,3.38761165659044));
#11446=CARTESIAN_POINT('Ctrl Pts',(-6.76301355578597,191.346893954693,3.2513674466916));
#11447=CARTESIAN_POINT('Ctrl Pts',(-6.82776836820671,191.281951283189,3.11307538412042));
#11448=CARTESIAN_POINT('Ctrl Pts',(-6.88817215625433,191.217273190527,2.97313145734446));
#11449=CARTESIAN_POINT('Ctrl Pts',(-6.94859215330858,191.152577741872,2.83314997742638));
#11450=CARTESIAN_POINT('Ctrl Pts',(-7.00465866845448,191.088147231024,2.69151625970926));
#11451=CARTESIAN_POINT('Ctrl Pts',(-7.05626368640816,191.024157275821,2.54864063860052));
#11452=CARTESIAN_POINT('Ctrl Pts',(-7.06221711430205,191.016775056042,2.53215775104821));
#11453=CARTESIAN_POINT('Ctrl Pts',(-7.06811121908795,191.009398692254,2.51565834512789));
#11454=CARTESIAN_POINT('Ctrl Pts',(-7.07394587853975,191.002028447915,2.49914305799789));
#11455=CARTESIAN_POINT('Ctrl Pts',(-7.12452344682944,190.938139708658,2.35598079299494));
#11456=CARTESIAN_POINT('Ctrl Pts',(-7.17087213616523,190.87379055128,2.21093899485705));
#11457=CARTESIAN_POINT('Ctrl Pts',(-7.21281294639898,190.809155844927,2.06440202409992));
#11458=CARTESIAN_POINT('Ctrl Pts',(-7.2563597607299,190.74204613624,1.91225383662786));
#11459=CARTESIAN_POINT('Ctrl Pts',(-7.29515405471514,190.674628800622,1.75849416561916));
#11460=CARTESIAN_POINT('Ctrl Pts',(-7.32904944559233,190.607105531561,1.60357741968119));
#11461=CARTESIAN_POINT('Ctrl Pts',(-7.36169037413291,190.542081286575,1.45439411472324));
#11462=CARTESIAN_POINT('Ctrl Pts',(-7.38978847549664,190.476959054234,1.30413842461194));
#11463=CARTESIAN_POINT('Ctrl Pts',(-7.41326423358634,190.411920847683,1.15323012442364));
#11464=CARTESIAN_POINT('Ctrl Pts',(-7.43673590800807,190.346893954693,1.00234807511892));
#11465=CARTESIAN_POINT('Ctrl Pts',(-7.45558679680081,190.281951283188,0.850814170351292));
#11466=CARTESIAN_POINT('Ctrl Pts',(-7.46978916139915,190.217273190524,0.69905378984192));
#11467=CARTESIAN_POINT('Ctrl Pts',(-7.48399533711969,190.15257774187,0.547252685314279));
#11468=CARTESIAN_POINT('Ctrl Pts',(-7.493550535944,190.088147231021,0.395225509155809));
#11469=CARTESIAN_POINT('Ctrl Pts',(-7.49847882953778,190.024157275818,0.243395891136868));
#11470=CARTESIAN_POINT('Ctrl Pts',(-7.49904738356042,190.01677505604,0.225880023131504));
#11471=CARTESIAN_POINT('Ctrl Pts',(-7.49955441349822,190.009398692253,0.208366777073135));
#11472=CARTESIAN_POINT('Ctrl Pts',(-7.5,190.002028447915,0.190856796705286));
#11473=CARTESIAN_POINT('Ctrl Pts',(-7.50386255306115,189.938139708658,0.0390720635508336));
#11474=CARTESIAN_POINT('Ctrl Pts',(-7.50312239555638,189.87379055128,-0.113193416375283));
#11475=CARTESIAN_POINT('Ctrl Pts',(-7.4977280621597,189.809155844927,-0.265518780412243));
#11476=CARTESIAN_POINT('Ctrl Pts',(-7.49212716810079,189.74204613624,-0.423677011229148));
#11477=CARTESIAN_POINT('Ctrl Pts',(-7.48150838279932,189.674628800622,-0.581899244411572));
#11478=CARTESIAN_POINT('Ctrl Pts',(-7.46587290795734,189.60710553156,-0.739708076931111));
#11479=CARTESIAN_POINT('Ctrl Pts',(-7.45081609923473,189.542081286575,-0.891676432865303));
#11480=CARTESIAN_POINT('Ctrl Pts',(-7.43110741988625,189.476959054234,-1.04326087688739));
#11481=CARTESIAN_POINT('Ctrl Pts',(-7.40680096324194,189.411920847682,-1.19403760735031));
#11482=CARTESIAN_POINT('Ctrl Pts',(-7.38249873476802,189.346893954693,-1.3447881098148));
#11483=CARTESIAN_POINT('Ctrl Pts',(-7.35360044359543,189.281951283189,-1.49473066237826));
#11484=CARTESIAN_POINT('Ctrl Pts',(-7.32021115834367,189.217273190526,-1.64345213319688));
#11485=CARTESIAN_POINT('Ctrl Pts',(-7.28681291327052,189.152577741871,-1.79221351256119));
#11486=CARTESIAN_POINT('Ctrl Pts',(-7.24892146633721,189.088147231023,-1.93975266792177));
#11487=CARTESIAN_POINT('Ctrl Pts',(-7.20669061985663,189.02415727582,-2.08567414197882));
#11488=CARTESIAN_POINT('Ctrl Pts',(-7.20181864597947,189.016775056041,-2.10250841524041));
#11489=CARTESIAN_POINT('Ctrl Pts',(-7.19688896944668,189.009398692253,-2.11932118289446));
#11490=CARTESIAN_POINT('Ctrl Pts',(-7.19190186588755,189.002028447915,-2.13611185762632));
#11491=CARTESIAN_POINT('Ctrl Pts',(-7.14867131011472,188.938139708658,-2.28166131170383));
#11492=CARTESIAN_POINT('Ctrl Pts',(-7.10091475754315,188.873790551281,-2.42624566734616));
#11493=CARTESIAN_POINT('Ctrl Pts',(-7.0487133154537,188.809155844928,-2.56944875671694));
#11494=CARTESIAN_POINT('Ctrl Pts',(-6.99451296753918,188.742046136241,-2.71813540129337));
#11495=CARTESIAN_POINT('Ctrl Pts',(-6.93552054364173,188.674628800623,-2.8653323020667));
#11496=CARTESIAN_POINT('Ctrl Pts',(-6.87188471229685,188.607105531561,-3.01058579312224));
#11497=CARTESIAN_POINT('Ctrl Pts',(-6.81060403165581,188.542081286576,-3.15046347852764));
#11498=CARTESIAN_POINT('Ctrl Pts',(-6.74501779444825,188.476959054235,-3.28853853492835));
#11499=CARTESIAN_POINT('Ctrl Pts',(-6.67530840839942,188.411920847683,-3.42442461876454));
#11500=CARTESIAN_POINT('Ctrl Pts',(-6.60561114847652,188.346893954694,-3.560287064869));
#11501=CARTESIAN_POINT('Ctrl Pts',(-6.53179244342476,188.281951283189,-3.69396084347412));
#11502=CARTESIAN_POINT('Ctrl Pts',(-6.4540798842,188.217273190526,-3.82508551083678));
#11503=CARTESIAN_POINT('Ctrl Pts',(-6.37634647125945,188.152577741871,-3.95624536474554));
#11504=CARTESIAN_POINT('Ctrl Pts',(-6.29471745739878,188.088147231022,-4.08485433881718));
#11505=CARTESIAN_POINT('Ctrl Pts',(-6.20946132033607,188.024157275818,-4.21058385833828));
#11506=CARTESIAN_POINT('Ctrl Pts',(-6.19962572130782,188.01677505604,-4.22508868089568));
#11507=CARTESIAN_POINT('Ctrl Pts',(-6.18974188939115,188.009398692253,-4.23955521930367));
#11508=CARTESIAN_POINT('Ctrl Pts',(-6.17981026821527,188.002028447915,-4.25398300016699));
#11509=CARTESIAN_POINT('Ctrl Pts',(-6.09371831161279,187.938139708658,-4.37904978050011));
#11510=CARTESIAN_POINT('Ctrl Pts',(-6.00362010807988,187.873790551281,-4.50180008775034));
#11511=CARTESIAN_POINT('Ctrl Pts',(-5.90972139815848,187.809155844928,-4.62186318631311));
#11512=CARTESIAN_POINT('Ctrl Pts',(-5.81222710407815,187.742046136241,-4.74652375991708));
#11513=CARTESIAN_POINT('Ctrl Pts',(-5.71063563106011,187.674628800624,-4.86828667005243));
#11514=CARTESIAN_POINT('Ctrl Pts',(-5.60522856176118,187.607105531562,-4.98676639589878));
#11515=CARTESIAN_POINT('Ctrl Pts',(-5.50372258919049,187.542081286576,-5.10086120834287));
#11516=CARTESIAN_POINT('Ctrl Pts',(-5.39867883198795,187.476959054235,-5.21191112857629));
#11517=CARTESIAN_POINT('Ctrl Pts',(-5.29039015693491,187.411920847684,-5.31960508912596));
#11518=CARTESIAN_POINT('Ctrl Pts',(-5.18212031897362,187.346893954694,-5.42728031603598));
#11519=CARTESIAN_POINT('Ctrl Pts',(-5.07060708921829,187.28195128319,-5.53160039987254));
#11520=CARTESIAN_POINT('Ctrl Pts',(-4.9561783027727,187.217273190527,-5.63229286773812));
#11521=CARTESIAN_POINT('Ctrl Pts',(-4.84171881002545,187.152577741872,-5.73301235584388));
#11522=CARTESIAN_POINT('Ctrl Pts',(-4.72434264585857,187.088147231023,-5.83010200617073));
#11523=CARTESIAN_POINT('Ctrl Pts',(-4.60440668292569,187.024157275821,-5.92333228977387));
#11524=CARTESIAN_POINT('Ctrl Pts',(-4.59057023570601,187.016775056042,-5.93408782853645));
#11525=CARTESIAN_POINT('Ctrl Pts',(-4.57669974673625,187.009398692254,-5.94479205212704));
#11526=CARTESIAN_POINT('Ctrl Pts',(-4.56279578422009,187.002028447915,-5.95544464740895));
#11527=CARTESIAN_POINT('Ctrl Pts',(-4.44226970733713,186.938139708658,-6.04778634614834));
#11528=CARTESIAN_POINT('Ctrl Pts',(-4.31864929275469,186.87379055128,-6.1366869496822));
#11529=CARTESIAN_POINT('Ctrl Pts',(-4.19224477495805,186.809155844927,-6.22185744482188));
#11530=CARTESIAN_POINT('Ctrl Pts',(-4.0609999554994,186.74204613624,-6.31028930194741));
#11531=CARTESIAN_POINT('Ctrl Pts',(-3.9267539145694,186.674628800622,-6.39469921942832));
#11532=CARTESIAN_POINT('Ctrl Pts',(-3.78989358567389,186.607105531561,-6.47480755900255));
#11533=CARTESIAN_POINT('Ctrl Pts',(-3.65809843300279,186.542081286575,-6.55195110329779));
#11534=CARTESIAN_POINT('Ctrl Pts',(-3.52387957064348,186.476959054235,-6.62510554744101));
#11535=CARTESIAN_POINT('Ctrl Pts',(-3.38761165659234,186.411920847683,-6.69406554949743));
#11536=CARTESIAN_POINT('Ctrl Pts',(-3.25136744669377,186.346893954695,-6.76301355578491));
#11537=CARTESIAN_POINT('Ctrl Pts',(-3.11307538412286,186.28195128319,-6.82776836820559));
#11538=CARTESIAN_POINT('Ctrl Pts',(-2.97313145734719,186.217273190528,-6.88817215625315));
#11539=CARTESIAN_POINT('Ctrl Pts',(-2.83314997742771,186.152577741873,-6.94859215330807));
#11540=CARTESIAN_POINT('Ctrl Pts',(-2.69151625970919,186.088147231024,-7.00465866845454));
#11541=CARTESIAN_POINT('Ctrl Pts',(-2.54864063859899,186.024157275821,-7.05626368640871));
#11542=CARTESIAN_POINT('Ctrl Pts',(-2.53215775104719,186.016775056042,-7.06221711430242));
#11543=CARTESIAN_POINT('Ctrl Pts',(-2.51565834512738,186.009398692254,-7.06811121908813));
#11544=CARTESIAN_POINT('Ctrl Pts',(-2.49914305799789,186.002028447915,-7.07394587853975));
#11545=CARTESIAN_POINT('Ctrl Pts',(-2.35598079299478,185.938139708658,-7.12452344682949));
#11546=CARTESIAN_POINT('Ctrl Pts',(-2.21093899485675,185.87379055128,-7.17087213616532));
#11547=CARTESIAN_POINT('Ctrl Pts',(-2.06440202409945,185.809155844927,-7.21281294639912));
#11548=CARTESIAN_POINT('Ctrl Pts',(-1.91225383662743,185.74204613624,-7.25635976073001));
#11549=CARTESIAN_POINT('Ctrl Pts',(-1.75849416561874,185.674628800622,-7.29515405471524));
#11550=CARTESIAN_POINT('Ctrl Pts',(-1.60357741968081,185.60710553156,-7.32904944559241));
#11551=CARTESIAN_POINT('Ctrl Pts',(-1.45439411472211,185.542081286575,-7.36169037413315));
#11552=CARTESIAN_POINT('Ctrl Pts',(-1.30413842461007,185.476959054234,-7.38978847549698));
#11553=CARTESIAN_POINT('Ctrl Pts',(-1.15323012442101,185.411920847682,-7.41326423358675));
#11554=CARTESIAN_POINT('Ctrl Pts',(-1.002348075116,185.346893954692,-7.43673590800846));
#11555=CARTESIAN_POINT('Ctrl Pts',(-0.850814170348105,185.281951283187,
-7.45558679680118));
#11556=CARTESIAN_POINT('Ctrl Pts',(-0.699053789838449,185.217273190523,
-7.46978916139948));
#11557=CARTESIAN_POINT('Ctrl Pts',(-0.547252685310788,185.152577741868,
-7.48399533711995));
#11558=CARTESIAN_POINT('Ctrl Pts',(-0.395225509152289,185.088147231019,
-7.49355053594419));
#11559=CARTESIAN_POINT('Ctrl Pts',(-0.243395891133334,185.024157275817,
-7.4984788295379));
#11560=CARTESIAN_POINT('Ctrl Pts',(-0.225880023129145,185.016775056039,
-7.49904738356049));
#11561=CARTESIAN_POINT('Ctrl Pts',(-0.208366777071962,185.009398692252,
-7.49955441349825));
#11562=CARTESIAN_POINT('Ctrl Pts',(-0.190856796705286,185.002028447915,
-7.5));
#11563=CARTESIAN_POINT('Ctrl Pts',(-0.0390720635516772,184.938139708658,
-7.50386255306113));
#11564=CARTESIAN_POINT('Ctrl Pts',(0.113193416373591,184.873790551281,-7.50312239555639));
#11565=CARTESIAN_POINT('Ctrl Pts',(0.265518780409704,184.809155844928,-7.49772806215979));
#11566=CARTESIAN_POINT('Ctrl Pts',(0.42367701122682,184.742046136241,-7.49212716810092));
#11567=CARTESIAN_POINT('Ctrl Pts',(0.581899244409438,184.674628800623,-7.48150838279949));
#11568=CARTESIAN_POINT('Ctrl Pts',(0.739708076929191,184.607105531561,-7.46587290795754));
#11569=CARTESIAN_POINT('Ctrl Pts',(0.891676432862843,184.542081286576,-7.45081609923501));
#11570=CARTESIAN_POINT('Ctrl Pts',(1.04326087688443,184.476959054235,-7.43110741988665));
#11571=CARTESIAN_POINT('Ctrl Pts',(1.19403760734682,184.411920847684,-7.4068009632425));
#11572=CARTESIAN_POINT('Ctrl Pts',(1.34478810981303,184.346893954694,-7.38249873476838));
#11573=CARTESIAN_POINT('Ctrl Pts',(1.49473066237817,184.281951283189,-7.35360044359548));
#11574=CARTESIAN_POINT('Ctrl Pts',(1.64345213319847,184.217273190525,-7.32021115834331));
#11575=CARTESIAN_POINT('Ctrl Pts',(1.79221351256205,184.152577741871,-7.28681291327029));
#11576=CARTESIAN_POINT('Ctrl Pts',(1.93975266792193,184.088147231022,-7.24892146633715));
#11577=CARTESIAN_POINT('Ctrl Pts',(2.08567414197828,184.02415727582,-7.20669061985679));
#11578=CARTESIAN_POINT('Ctrl Pts',(2.10250841524006,184.016775056042,-7.20181864597957));
#11579=CARTESIAN_POINT('Ctrl Pts',(2.11932118289428,184.009398692253,-7.19688896944673));
#11580=CARTESIAN_POINT('Ctrl Pts',(2.13611185762632,184.002028447915,-7.19190186588755));
#11581=CARTESIAN_POINT('Ctrl Pts',(2.28166131170458,183.938139708658,-7.14867131011449));
#11582=CARTESIAN_POINT('Ctrl Pts',(2.42624566734765,183.87379055128,-7.10091475754266));
#11583=CARTESIAN_POINT('Ctrl Pts',(2.56944875671915,183.809155844927,-7.0487133154529));
#11584=CARTESIAN_POINT('Ctrl Pts',(2.71813540129538,183.74204613624,-6.9945129675384));
#11585=CARTESIAN_POINT('Ctrl Pts',(2.86533230206852,183.674628800622,-6.93552054364098));
#11586=CARTESIAN_POINT('Ctrl Pts',(3.01058579312386,183.60710553156,-6.87188471229614));
#11587=CARTESIAN_POINT('Ctrl Pts',(3.15046347852959,183.542081286575,-6.81060403165491));
#11588=CARTESIAN_POINT('Ctrl Pts',(3.28853853493061,183.476959054234,-6.74501779444716));
#11589=CARTESIAN_POINT('Ctrl Pts',(3.4244246187671,183.411920847682,-6.6753084083981));
#11590=CARTESIAN_POINT('Ctrl Pts',(3.5602870648721,183.346893954692,-6.60561114847487));
#11591=CARTESIAN_POINT('Ctrl Pts',(3.69396084347772,183.281951283188,-6.53179244342274));
#11592=CARTESIAN_POINT('Ctrl Pts',(3.82508551084086,183.217273190524,-6.45407988419758));
#11593=CARTESIAN_POINT('Ctrl Pts',(3.95624536474775,183.15257774187,-6.37634647125802));
#11594=CARTESIAN_POINT('Ctrl Pts',(4.08485433881761,183.088147231021,-6.29471745739845));
#11595=CARTESIAN_POINT('Ctrl Pts',(4.21058385833698,183.024157275819,-6.20946132033695));
#11596=CARTESIAN_POINT('Ctrl Pts',(4.22508868089482,183.016775056041,-6.19962572130841));
#11597=CARTESIAN_POINT('Ctrl Pts',(4.23955521930325,183.009398692253,-6.18974188939143));
#11598=CARTESIAN_POINT('Ctrl Pts',(4.25398300016701,183.002028447915,-6.17981026821526));
#11599=CARTESIAN_POINT('Ctrl Pts',(4.37904978050103,182.938139708658,-6.09371831161216));
#11600=CARTESIAN_POINT('Ctrl Pts',(4.50180008775213,182.87379055128,-6.00362010807857));
#11601=CARTESIAN_POINT('Ctrl Pts',(4.62186318631574,182.809155844927,-5.90972139815642));
#11602=CARTESIAN_POINT('Ctrl Pts',(4.74652375991945,182.74204613624,-5.81222710407621));
#11603=CARTESIAN_POINT('Ctrl Pts',(4.86828667005454,182.674628800622,-5.7106356310583));
#11604=CARTESIAN_POINT('Ctrl Pts',(4.98676639590065,182.607105531561,-5.60522856175951));
#11605=CARTESIAN_POINT('Ctrl Pts',(5.10086120834469,182.542081286575,-5.5037225891888));
#11606=CARTESIAN_POINT('Ctrl Pts',(5.21191112857806,182.476959054234,-5.39867883198624));
#11607=CARTESIAN_POINT('Ctrl Pts',(5.31960508912767,182.411920847683,-5.29039015693319));
#11608=CARTESIAN_POINT('Ctrl Pts',(5.42728031603767,182.346893954693,-5.18212031897185));
#11609=CARTESIAN_POINT('Ctrl Pts',(5.53160039987421,182.281951283189,-5.07060708921647));
#11610=CARTESIAN_POINT('Ctrl Pts',(5.63229286773977,182.217273190526,-4.95617830277083));
#11611=CARTESIAN_POINT('Ctrl Pts',(5.73301235584584,182.152577741871,-4.84171881002315));
#11612=CARTESIAN_POINT('Ctrl Pts',(5.83010200617298,182.088147231022,-4.72434264585582));
#11613=CARTESIAN_POINT('Ctrl Pts',(5.92333228977637,182.024157275819,-4.60440668292248));
#11614=CARTESIAN_POINT('Ctrl Pts',(5.9340878285381,182.016775056041,-4.59057023570386));
#11615=CARTESIAN_POINT('Ctrl Pts',(5.94479205212786,182.009398692253,-4.57669974673518));
#11616=CARTESIAN_POINT('Ctrl Pts',(5.95544464740895,182.002028447915,-4.56279578422009));
#11617=CARTESIAN_POINT('Ctrl Pts',(6.04778634614845,181.938139708658,-4.442269707337));
#11618=CARTESIAN_POINT('Ctrl Pts',(6.1366869496824,181.87379055128,-4.3186492927544));
#11619=CARTESIAN_POINT('Ctrl Pts',(6.22185744482218,181.809155844927,-4.19224477495761));
#11620=CARTESIAN_POINT('Ctrl Pts',(6.31028930194767,181.74204613624,-4.06099995549899));
#11621=CARTESIAN_POINT('Ctrl Pts',(6.39469921942856,181.674628800622,-3.92675391456902));
#11622=CARTESIAN_POINT('Ctrl Pts',(6.47480755900275,181.60710553156,-3.78989358567354));
#11623=CARTESIAN_POINT('Ctrl Pts',(6.5519511032983,181.542081286575,-3.65809843300192));
#11624=CARTESIAN_POINT('Ctrl Pts',(6.62510554744178,181.476959054234,-3.52387957064205));
#11625=CARTESIAN_POINT('Ctrl Pts',(6.69406554949843,181.411920847682,-3.38761165659035));
#11626=CARTESIAN_POINT('Ctrl Pts',(6.76301355578636,181.346893954693,-3.25136744669082));
#11627=CARTESIAN_POINT('Ctrl Pts',(6.8277683682074,181.281951283189,-3.11307538411894));
#11628=CARTESIAN_POINT('Ctrl Pts',(6.88817215625527,181.217273190526,-2.97313145734227));
#11629=CARTESIAN_POINT('Ctrl Pts',(6.94859215331014,181.152577741871,-2.83314997742263));
#11630=CARTESIAN_POINT('Ctrl Pts',(7.00465866845655,181.088147231021,-2.69151625970395));
#11631=CARTESIAN_POINT('Ctrl Pts',(7.05626368641066,181.024157275818,-2.54864063859361));
#11632=CARTESIAN_POINT('Ctrl Pts',(7.0622171143037,181.01677505604,-2.5321577510436));
#11633=CARTESIAN_POINT('Ctrl Pts',(7.06811121908876,181.009398692253,-2.51565834512559));
#11634=CARTESIAN_POINT('Ctrl Pts',(7.07394587853975,181.002028447915,-2.4991430579979));
#11635=CARTESIAN_POINT('Ctrl Pts',(7.12452344682943,180.938139708658,-2.35598079299495));
#11636=CARTESIAN_POINT('Ctrl Pts',(7.17087213616523,180.87379055128,-2.21093899485704));
#11637=CARTESIAN_POINT('Ctrl Pts',(7.21281294639899,180.809155844927,-2.0644020240999));
#11638=CARTESIAN_POINT('Ctrl Pts',(7.2563597607299,180.74204613624,-1.91225383662784));
#11639=CARTESIAN_POINT('Ctrl Pts',(7.29515405471515,180.674628800622,-1.75849416561912));
#11640=CARTESIAN_POINT('Ctrl Pts',(7.32904944559233,180.607105531561,-1.60357741968115));
#11641=CARTESIAN_POINT('Ctrl Pts',(7.36169037413299,180.542081286575,-1.45439411472287));
#11642=CARTESIAN_POINT('Ctrl Pts',(7.38978847549676,180.476959054234,-1.30413842461125));
#11643=CARTESIAN_POINT('Ctrl Pts',(7.4132642335865,180.411920847682,-1.15323012442261));
#11644=CARTESIAN_POINT('Ctrl Pts',(7.43673590800803,180.346893954693,-1.00234807511903));
#11645=CARTESIAN_POINT('Ctrl Pts',(7.45558679680064,180.281951283189,-0.850814170352573));
#11646=CARTESIAN_POINT('Ctrl Pts',(7.46978916139892,180.217273190526,-0.699053789844363));
#11647=CARTESIAN_POINT('Ctrl Pts',(7.48399533711951,180.152577741871,-0.547252685316772));
#11648=CARTESIAN_POINT('Ctrl Pts',(7.49355053594387,180.088147231022,-0.39522550915836));
#11649=CARTESIAN_POINT('Ctrl Pts',(7.4984788295377,180.024157275819,-0.243395891139465));
#11650=CARTESIAN_POINT('Ctrl Pts',(7.49904738356037,180.016775056041,-0.225880023133238));
#11651=CARTESIAN_POINT('Ctrl Pts',(7.49955441349819,180.009398692253,-0.208366777073998));
#11652=CARTESIAN_POINT('Ctrl Pts',(7.5,180.002028447915,-0.190856796705287));
#11653=CARTESIAN_POINT('Ctrl Pts',(7.50386255306115,179.938139708658,-0.0390720635508177));
#11654=CARTESIAN_POINT('Ctrl Pts',(7.50312239555638,179.87379055128,0.113193416375312));
#11655=CARTESIAN_POINT('Ctrl Pts',(7.49772806215969,179.809155844927,0.265518780412289));
#11656=CARTESIAN_POINT('Ctrl Pts',(7.49212716810078,179.74204613624,0.42367701122919));
#11657=CARTESIAN_POINT('Ctrl Pts',(7.48150838279932,179.674628800622,0.581899244411606));
#11658=CARTESIAN_POINT('Ctrl Pts',(7.46587290795734,179.60710553156,0.739708076931141));
#11659=CARTESIAN_POINT('Ctrl Pts',(7.45081609923473,179.542081286575,0.891676432865285));
#11660=CARTESIAN_POINT('Ctrl Pts',(7.43110741988625,179.476959054234,1.04326087688732));
#11661=CARTESIAN_POINT('Ctrl Pts',(7.40680096324196,179.411920847682,1.1940376073502));
#11662=CARTESIAN_POINT('Ctrl Pts',(7.38249873476815,179.346893954694,1.34478810981401));
#11663=CARTESIAN_POINT('Ctrl Pts',(7.35360044359571,179.281951283189,1.4947306623768));
#11664=CARTESIAN_POINT('Ctrl Pts',(7.32021115834415,179.217273190527,1.64345213319477));
#11665=CARTESIAN_POINT('Ctrl Pts',(7.28681291327109,179.152577741872,1.79221351255885));
#11666=CARTESIAN_POINT('Ctrl Pts',(7.24892146633789,179.088147231024,1.93975266791923));
#11667=CARTESIAN_POINT('Ctrl Pts',(7.20669061985743,179.024157275821,2.08567414197607));
#11668=CARTESIAN_POINT('Ctrl Pts',(7.20181864598001,179.016775056042,2.10250841523858));
#11669=CARTESIAN_POINT('Ctrl Pts',(7.19688896944695,179.009398692254,2.11932118289354));
#11670=CARTESIAN_POINT('Ctrl Pts',(7.19190186588755,179.002028447915,2.13611185762632));
#11671=CARTESIAN_POINT('Ctrl Pts',(7.14867131011455,178.938139708658,2.2816613117044));
#11672=CARTESIAN_POINT('Ctrl Pts',(7.10091475754278,178.87379055128,2.42624566734728));
#11673=CARTESIAN_POINT('Ctrl Pts',(7.0487133154531,178.809155844927,2.56944875671861));
#11674=CARTESIAN_POINT('Ctrl Pts',(6.99451296753859,178.74204613624,2.71813540129489));
#11675=CARTESIAN_POINT('Ctrl Pts',(6.93552054364116,178.674628800623,2.86533230206808));
#11676=CARTESIAN_POINT('Ctrl Pts',(6.87188471229631,178.607105531561,3.01058579312346));
#11677=CARTESIAN_POINT('Ctrl Pts',(6.81060403165535,178.542081286575,3.15046347852861));
#11678=CARTESIAN_POINT('Ctrl Pts',(6.7450177944479,178.476959054234,3.28853853492906));
#11679=CARTESIAN_POINT('Ctrl Pts',(6.67530840839917,178.411920847683,3.42442461876501));
#11680=CARTESIAN_POINT('Ctrl Pts',(6.60561114847623,178.346893954694,3.56028706486955));
#11681=CARTESIAN_POINT('Ctrl Pts',(6.53179244342441,178.281951283189,3.69396084347474));
#11682=CARTESIAN_POINT('Ctrl Pts',(6.4540798841996,178.217273190526,3.82508551083747));
#11683=CARTESIAN_POINT('Ctrl Pts',(6.37634647126001,178.152577741872,3.95624536474455));
#11684=CARTESIAN_POINT('Ctrl Pts',(6.29471745740041,178.088147231023,4.08485433881459));
#11685=CARTESIAN_POINT('Ctrl Pts',(6.20946132033887,178.02415727582,4.21058385833414));
#11686=CARTESIAN_POINT('Ctrl Pts',(6.1996257213097,178.016775056042,4.22508868089293));
#11687=CARTESIAN_POINT('Ctrl Pts',(6.18974188939208,178.009398692254,4.23955521930231));
#11688=CARTESIAN_POINT('Ctrl Pts',(6.17981026821526,178.002028447915,4.25398300016701));
#11689=CARTESIAN_POINT('Ctrl Pts',(6.09371831161207,177.938139708658,4.37904978050116));
#11690=CARTESIAN_POINT('Ctrl Pts',(6.0036201080784,177.87379055128,4.50180008775236));
#11691=CARTESIAN_POINT('Ctrl Pts',(5.90972139815616,177.809155844927,4.62186318631608));
#11692=CARTESIAN_POINT('Ctrl Pts',(5.81222710407596,177.74204613624,4.74652375991976));
#11693=CARTESIAN_POINT('Ctrl Pts',(5.71063563105806,177.674628800622,4.86828667005482));
#11694=CARTESIAN_POINT('Ctrl Pts',(5.6052285617593,177.60710553156,4.98676639590089));
#11695=CARTESIAN_POINT('Ctrl Pts',(5.5037225891889,177.542081286575,5.10086120834457));
#11696=CARTESIAN_POINT('Ctrl Pts',(5.39867883198667,177.476959054235,5.2119111285776));
#11697=CARTESIAN_POINT('Ctrl Pts',(5.29039015693398,177.411920847683,5.31960508912689));
#11698=CARTESIAN_POINT('Ctrl Pts',(5.18212031897253,177.346893954694,5.42728031603702));
#11699=CARTESIAN_POINT('Ctrl Pts',(5.07060708921705,177.281951283189,5.53160039987369));
#11700=CARTESIAN_POINT('Ctrl Pts',(4.95617830277129,177.217273190526,5.63229286773936));
#11701=CARTESIAN_POINT('Ctrl Pts',(4.84171881002452,177.152577741872,5.73301235584465));
#11702=CARTESIAN_POINT('Ctrl Pts',(4.72434264585812,177.088147231023,5.83010200617108));
#11703=CARTESIAN_POINT('Ctrl Pts',(4.60440668292578,177.024157275821,5.92333228977381));
#11704=CARTESIAN_POINT('Ctrl Pts',(4.59057023570606,177.016775056042,5.93408782853641));
#11705=CARTESIAN_POINT('Ctrl Pts',(4.57669974673629,177.009398692254,5.94479205212701));
#11706=CARTESIAN_POINT('Ctrl Pts',(4.56279578422009,177.002028447915,5.95544464740895));
#11707=CARTESIAN_POINT('Ctrl Pts',(4.44226970733713,176.938139708658,6.04778634614834));
#11708=CARTESIAN_POINT('Ctrl Pts',(4.31864929275468,176.87379055128,6.1366869496822));
#11709=CARTESIAN_POINT('Ctrl Pts',(4.19224477495804,176.809155844927,6.22185744482189));
#11710=CARTESIAN_POINT('Ctrl Pts',(4.06099995549939,176.74204613624,6.31028930194742));
#11711=CARTESIAN_POINT('Ctrl Pts',(3.92675391456939,176.674628800622,6.39469921942833));
#11712=CARTESIAN_POINT('Ctrl Pts',(3.78989358567388,176.607105531561,6.47480755900255));
#11713=CARTESIAN_POINT('Ctrl Pts',(3.65809843300261,176.542081286575,6.5519511032979));
#11714=CARTESIAN_POINT('Ctrl Pts',(3.52387957064311,176.476959054234,6.62510554744121));
#11715=CARTESIAN_POINT('Ctrl Pts',(3.38761165659179,176.411920847683,6.69406554949771));
#11716=CARTESIAN_POINT('Ctrl Pts',(3.25136744669221,176.346893954694,6.76301355578569));
#11717=CARTESIAN_POINT('Ctrl Pts',(3.11307538412028,176.281951283189,6.82776836820679));
#11718=CARTESIAN_POINT('Ctrl Pts',(2.97313145734355,176.217273190526,6.88817215625472));
#11719=CARTESIAN_POINT('Ctrl Pts',(2.83314997742486,176.152577741872,6.94859215330921));
#11720=CARTESIAN_POINT('Ctrl Pts',(2.69151625970714,176.088147231023,7.00465866845531));
#11721=CARTESIAN_POINT('Ctrl Pts',(2.54864063859777,176.02415727582,7.05626368640916));
#11722=CARTESIAN_POINT('Ctrl Pts',(2.53215775104638,176.016775056042,7.06221711430271));
#11723=CARTESIAN_POINT('Ctrl Pts',(2.51565834512697,176.009398692253,7.06811121908827));
#11724=CARTESIAN_POINT('Ctrl Pts',(2.49914305799789,176.002028447915,7.07394587853975));
#11725=CARTESIAN_POINT('Ctrl Pts',(2.35598079328146,175.938139708785,7.12452344672821));
#11726=CARTESIAN_POINT('Ctrl Pts',(2.21093899543762,175.873790551538,7.17087213597972));
#11727=CARTESIAN_POINT('Ctrl Pts',(2.06440202497974,175.809155845315,7.21281294614716));
#11728=CARTESIAN_POINT('Ctrl Pts',(1.91225491695072,175.742046612748,7.25635945154735));
#11729=CARTESIAN_POINT('Ctrl Pts',(1.75849634827299,175.674629757621,7.2951535041046));
#11730=CARTESIAN_POINT('Ctrl Pts',(1.60358071781314,175.607106969111,7.32904872396865));
#11731=CARTESIAN_POINT('Ctrl Pts',(1.4543974295954,175.542082725982,7.36168971919407));
#11732=CARTESIAN_POINT('Ctrl Pts',(1.30414175318146,175.476960494159,7.38978788807506));
#11733=CARTESIAN_POINT('Ctrl Pts',(1.15323346356763,175.411922286781,7.41326371413808));
#11734=CARTESIAN_POINT('Ctrl Pts',(1.0023514247394,175.346895392924,7.43673545653627));
#11735=CARTESIAN_POINT('Ctrl Pts',(0.850817527325577,175.281952719209,7.45558641375475));
#11736=CARTESIAN_POINT('Ctrl Pts',(0.699057151026253,175.217274623013,7.46978884684485));
#11737=CARTESIAN_POINT('Ctrl Pts',(0.547256052215635,175.152579171467,7.4839950909346));
#11738=CARTESIAN_POINT('Ctrl Pts',(0.395228878633319,175.088148656398,7.49355035828583));
#11739=CARTESIAN_POINT('Ctrl Pts',(0.243399260074249,175.024158695687,7.49847872018344));
#11740=CARTESIAN_POINT('Ctrl Pts',(0.225886742935279,175.016777887553,7.49904717331543));
#11741=CARTESIAN_POINT('Ctrl Pts',(0.208376846698734,175.009402933151,7.49955412589778));
#11742=CARTESIAN_POINT('Ctrl Pts',(0.190870214739035,175.002034095791,7.4999996585316));
#11743=CARTESIAN_POINT('',(0.000256710970817156,177.995967593475,7.49999999788466));
#11744=CARTESIAN_POINT('Origin',(-5.20512090547431E-6,178.000081808606,
-1851.55088195117));
#11745=CARTESIAN_POINT('',(-1.89809114034451E-16,197.99585953923,7.50000000439337));
#11746=CARTESIAN_POINT('Ctrl Pts',(5.38866871829646E-16,197.99585953923,
7.50000000439337));
#11747=CARTESIAN_POINT('Ctrl Pts',(-1.18775172812192,197.495912211348,7.50000000439337));
#11748=CARTESIAN_POINT('Ctrl Pts',(-2.317383311169,196.995967593475,7.13300320026677));
#11749=CARTESIAN_POINT('Ctrl Pts',(-3.44714003087638,196.495967593475,6.76596574150984));
#11750=CARTESIAN_POINT('Ctrl Pts',(-4.40818170865423,195.995967593475,6.06777834873578));
#11751=CARTESIAN_POINT('Ctrl Pts',(-5.36922338643209,195.495967593475,5.36959095596173));
#11752=CARTESIAN_POINT('Ctrl Pts',(-6.06747656688843,194.995967593475,4.40859707573286));
#11753=CARTESIAN_POINT('Ctrl Pts',(-6.76572974734476,194.495967593475,3.447603195504));
#11754=CARTESIAN_POINT('Ctrl Pts',(-7.13284454416054,193.995967593475,2.31787160445521));
#11755=CARTESIAN_POINT('Ctrl Pts',(-7.49995934097631,193.495967593475,1.18814001340642));
#11756=CARTESIAN_POINT('Ctrl Pts',(-7.5,192.995967593475,0.000256710972401669));
#11757=CARTESIAN_POINT('Ctrl Pts',(-7.50004065902369,192.495967593475,-1.18762659146162));
#11758=CARTESIAN_POINT('Ctrl Pts',(-7.13300320026677,191.995967593475,-2.317383311169));
#11759=CARTESIAN_POINT('Ctrl Pts',(-6.76596574150984,191.495967593475,-3.44714003087638));
#11760=CARTESIAN_POINT('Ctrl Pts',(-6.06777834873578,190.995967593475,-4.40818170865423));
#11761=CARTESIAN_POINT('Ctrl Pts',(-5.36959095596173,190.495967593475,-5.36922338643209));
#11762=CARTESIAN_POINT('Ctrl Pts',(-4.40859707573286,189.995967593475,-6.06747656688843));
#11763=CARTESIAN_POINT('Ctrl Pts',(-3.447603195504,189.495967593475,-6.76572974734476));
#11764=CARTESIAN_POINT('Ctrl Pts',(-2.31787160445521,188.995967593475,-7.13284454416054));
#11765=CARTESIAN_POINT('Ctrl Pts',(-1.18814001340642,188.495967593475,-7.49995934097631));
#11766=CARTESIAN_POINT('Ctrl Pts',(-0.000256710972402128,187.995967593475,
-7.5));
#11767=CARTESIAN_POINT('Ctrl Pts',(1.18762659146162,187.495967593475,-7.50004065902369));
#11768=CARTESIAN_POINT('Ctrl Pts',(2.317383311169,186.995967593475,-7.13300320026677));
#11769=CARTESIAN_POINT('Ctrl Pts',(3.44714003087638,186.495967593475,-6.76596574150984));
#11770=CARTESIAN_POINT('Ctrl Pts',(4.40818170865423,185.995967593475,-6.06777834873578));
#11771=CARTESIAN_POINT('Ctrl Pts',(5.36922338643209,185.495967593475,-5.36959095596173));
#11772=CARTESIAN_POINT('Ctrl Pts',(6.06747656688843,184.995967593475,-4.40859707573286));
#11773=CARTESIAN_POINT('Ctrl Pts',(6.76572974734476,184.495967593475,-3.447603195504));
#11774=CARTESIAN_POINT('Ctrl Pts',(7.13284454416054,183.995967593475,-2.31787160445521));
#11775=CARTESIAN_POINT('Ctrl Pts',(7.49995934097631,183.495967593475,-1.18814001340642));
#11776=CARTESIAN_POINT('Ctrl Pts',(7.5,182.995967593475,-0.000256710972402588));
#11777=CARTESIAN_POINT('Ctrl Pts',(7.50004065902369,182.495967593475,1.18762659146162));
#11778=CARTESIAN_POINT('Ctrl Pts',(7.13300320026677,181.995967593475,2.317383311169));
#11779=CARTESIAN_POINT('Ctrl Pts',(6.76596574150984,181.495967593475,3.44714003087638));
#11780=CARTESIAN_POINT('Ctrl Pts',(6.06777834873579,180.995967593475,4.40818170865423));
#11781=CARTESIAN_POINT('Ctrl Pts',(5.36959095596173,180.495967593475,5.36922338643209));
#11782=CARTESIAN_POINT('Ctrl Pts',(4.40859707573286,179.995967593475,6.06747656688843));
#11783=CARTESIAN_POINT('Ctrl Pts',(3.447603195504,179.495967593475,6.76572974734476));
#11784=CARTESIAN_POINT('Ctrl Pts',(2.31787160445521,178.995967593475,7.13284454416054));
#11785=CARTESIAN_POINT('Ctrl Pts',(1.18814001340643,178.495967593475,7.49995934097631));
#11786=CARTESIAN_POINT('Ctrl Pts',(0.00025671097240121,177.995967593475,
7.5));
#11787=CARTESIAN_POINT('',(-4.06843942354914E-7,214.921557632927,7.50242802810186));
#11788=CARTESIAN_POINT('',(-9.18485099360515E-16,240.,7.5));
#11789=CARTESIAN_POINT('Ctrl Pts',(-4.068439266928E-7,214.921557632927,
7.50242802810187));
#11790=CARTESIAN_POINT('Ctrl Pts',(-0.152090385416069,214.857323985265,
7.50242801985428));
#11791=CARTESIAN_POINT('Ctrl Pts',(-0.304485788638696,214.792702491972,
7.49779895914527));
#11792=CARTESIAN_POINT('Ctrl Pts',(-0.456762644215681,214.72787053402,7.48851081348606));
#11793=CARTESIAN_POINT('Ctrl Pts',(-0.609070650331504,214.663025313709,
7.47922076779588));
#11794=CARTESIAN_POINT('Ctrl Pts',(-0.761259533138804,214.597969762788,
7.46526968655064));
#11795=CARTESIAN_POINT('Ctrl Pts',(-0.91290272043933,214.532885263597,7.44667945730599));
#11796=CARTESIAN_POINT('Ctrl Pts',(-1.0645049306871,214.467818351553,7.42809425151685));
#11797=CARTESIAN_POINT('Ctrl Pts',(-1.21556121279854,214.402722732839,7.40487246128572));
#11798=CARTESIAN_POINT('Ctrl Pts',(-1.36565093134601,214.3377801784,7.37708776215671));
#11799=CARTESIAN_POINT('Ctrl Pts',(-1.51579830432504,214.272812677376,7.3492923900046));
#11800=CARTESIAN_POINT('Ctrl Pts',(-1.66497786162516,214.207998581557,7.31693074896066));
#11801=CARTESIAN_POINT('Ctrl Pts',(-1.8127818777126,214.143517028959,7.28012693438002));
#11802=CARTESIAN_POINT('Ctrl Pts',(-1.92135204017723,214.096151789321,7.25309251248735));
#11803=CARTESIAN_POINT('Ctrl Pts',(-2.02918025203189,214.04896593395,7.22366229239569));
#11804=CARTESIAN_POINT('Ctrl Pts',(-2.13611185762632,214.002028447915,7.19190186588755));
#11805=CARTESIAN_POINT('Ctrl Pts',(-2.28166131170438,213.938139708658,7.14867131011455));
#11806=CARTESIAN_POINT('Ctrl Pts',(-2.42624566734726,213.87379055128,7.10091475754279));
#11807=CARTESIAN_POINT('Ctrl Pts',(-2.56944875671857,213.809155844927,7.04871331545311));
#11808=CARTESIAN_POINT('Ctrl Pts',(-2.71813540129485,213.74204613624,6.99451296753861));
#11809=CARTESIAN_POINT('Ctrl Pts',(-2.86533230206802,213.674628800623,6.93552054364118));
#11810=CARTESIAN_POINT('Ctrl Pts',(-3.01058579312341,213.607105531561,6.87188471229634));
#11811=CARTESIAN_POINT('Ctrl Pts',(-3.15046347852853,213.542081286575,6.81060403165539));
#11812=CARTESIAN_POINT('Ctrl Pts',(-3.28853853492897,213.476959054234,6.74501779444794));
#11813=CARTESIAN_POINT('Ctrl Pts',(-3.4244246187649,213.411920847683,6.67530840839923));
#11814=CARTESIAN_POINT('Ctrl Pts',(-3.56028706486959,213.346893954694,6.60561114847621));
#11815=CARTESIAN_POINT('Ctrl Pts',(-3.69396084347493,213.281951283189,6.53179244342431));
#11816=CARTESIAN_POINT('Ctrl Pts',(-3.8250855108378,213.217273190526,6.4540798841994));
#11817=CARTESIAN_POINT('Ctrl Pts',(-3.95624536474509,213.152577741871,6.37634647125968));
#11818=CARTESIAN_POINT('Ctrl Pts',(-4.08485433881534,213.088147231023,6.29471745739993));
#11819=CARTESIAN_POINT('Ctrl Pts',(-4.21058385833508,213.02415727582,6.20946132033823));
#11820=CARTESIAN_POINT('Ctrl Pts',(-4.22508868089356,213.016775056042,6.19962572130926));
#11821=CARTESIAN_POINT('Ctrl Pts',(-4.23955521930262,213.009398692253,6.18974188939186));
#11822=CARTESIAN_POINT('Ctrl Pts',(-4.25398300016701,213.002028447915,6.17981026821525));
#11823=CARTESIAN_POINT('Ctrl Pts',(-4.37904978050102,212.938139708658,6.09371831161217));
#11824=CARTESIAN_POINT('Ctrl Pts',(-4.50180008775209,212.87379055128,6.00362010807859));
#11825=CARTESIAN_POINT('Ctrl Pts',(-4.62186318631568,212.809155844927,5.90972139815647));
#11826=CARTESIAN_POINT('Ctrl Pts',(-4.74652375991939,212.74204613624,5.81222710407626));
#11827=CARTESIAN_POINT('Ctrl Pts',(-4.86828667005449,212.674628800623,5.71063563105834));
#11828=CARTESIAN_POINT('Ctrl Pts',(-4.9867663959006,212.607105531561,5.60522856175955));
#11829=CARTESIAN_POINT('Ctrl Pts',(-5.10086120834463,212.542081286575,5.50372258918886));
#11830=CARTESIAN_POINT('Ctrl Pts',(-5.21191112857799,212.476959054234,5.39867883198632));
#11831=CARTESIAN_POINT('Ctrl Pts',(-5.31960508912758,212.411920847683,5.29039015693328));
#11832=CARTESIAN_POINT('Ctrl Pts',(-5.42728031603771,212.346893954693,5.18212031897182));
#11833=CARTESIAN_POINT('Ctrl Pts',(-5.53160039987437,212.281951283189,5.07060708921631));
#11834=CARTESIAN_POINT('Ctrl Pts',(-5.63229286774003,212.217273190525,4.95617830277053));
#11835=CARTESIAN_POINT('Ctrl Pts',(-5.73301235584579,212.152577741871,4.84171881002319));
#11836=CARTESIAN_POINT('Ctrl Pts',(-5.83010200617264,212.088147231022,4.72434264585622));
#11837=CARTESIAN_POINT('Ctrl Pts',(-5.92333228977576,212.02415727582,4.60440668292327));
#11838=CARTESIAN_POINT('Ctrl Pts',(-5.9340878285377,212.016775056041,4.59057023570439));
#11839=CARTESIAN_POINT('Ctrl Pts',(-5.94479205212766,212.009398692253,4.57669974673545));
#11840=CARTESIAN_POINT('Ctrl Pts',(-5.95544464740895,212.002028447915,4.5627957842201));
#11841=CARTESIAN_POINT('Ctrl Pts',(-6.04778634614838,211.938139708658,4.44226970733709));
#11842=CARTESIAN_POINT('Ctrl Pts',(-6.13668694968226,211.87379055128,4.3186492927546));
#11843=CARTESIAN_POINT('Ctrl Pts',(-6.22185744482198,211.809155844927,4.19224477495791));
#11844=CARTESIAN_POINT('Ctrl Pts',(-6.3102893019475,211.74204613624,4.06099995549926));
#11845=CARTESIAN_POINT('Ctrl Pts',(-6.39469921942841,211.674628800622,3.92675391456926));
#11846=CARTESIAN_POINT('Ctrl Pts',(-6.47480755900262,211.607105531561,3.78989358567376));
#11847=CARTESIAN_POINT('Ctrl Pts',(-6.55195110329808,211.542081286575,3.65809843300229));
#11848=CARTESIAN_POINT('Ctrl Pts',(-6.62510554744149,211.476959054234,3.52387957064258));
#11849=CARTESIAN_POINT('Ctrl Pts',(-6.69406554949808,211.411920847683,3.38761165659104));
#11850=CARTESIAN_POINT('Ctrl Pts',(-6.76301355578619,211.346893954693,3.25136744669118));
#11851=CARTESIAN_POINT('Ctrl Pts',(-6.8277683682074,211.281951283189,3.11307538411895));
#11852=CARTESIAN_POINT('Ctrl Pts',(-6.88817215625542,211.217273190525,2.97313145734192));
#11853=CARTESIAN_POINT('Ctrl Pts',(-6.94859215330986,211.152577741871,2.83314997742328));
#11854=CARTESIAN_POINT('Ctrl Pts',(-7.00465866845589,211.088147231022,2.69151625970561));
#11855=CARTESIAN_POINT('Ctrl Pts',(-7.05626368640969,211.02415727582,2.5486406385963));
#11856=CARTESIAN_POINT('Ctrl Pts',(-7.06221711430306,211.016775056041,2.53215775104539));
#11857=CARTESIAN_POINT('Ctrl Pts',(-7.06811121908845,211.009398692253,2.51565834512648));
#11858=CARTESIAN_POINT('Ctrl Pts',(-7.07394587853975,211.002028447915,2.49914305799789));
#11859=CARTESIAN_POINT('Ctrl Pts',(-7.12452344682943,210.938139708658,2.35598079299496));
#11860=CARTESIAN_POINT('Ctrl Pts',(-7.17087213616521,210.87379055128,2.2109389948571));
#11861=CARTESIAN_POINT('Ctrl Pts',(-7.21281294639896,210.809155844927,2.06440202409999));
#11862=CARTESIAN_POINT('Ctrl Pts',(-7.25635976072988,210.74204613624,1.91225383662793));
#11863=CARTESIAN_POINT('Ctrl Pts',(-7.29515405471512,210.674628800622,1.75849416561922));
#11864=CARTESIAN_POINT('Ctrl Pts',(-7.32904944559231,210.607105531561,1.60357741968125));
#11865=CARTESIAN_POINT('Ctrl Pts',(-7.3616903741329,210.542081286575,1.4543941147233));
#11866=CARTESIAN_POINT('Ctrl Pts',(-7.38978847549662,210.476959054234,1.30413842461201));
#11867=CARTESIAN_POINT('Ctrl Pts',(-7.41326423358633,210.411920847683,1.15323012442371));
#11868=CARTESIAN_POINT('Ctrl Pts',(-7.43673590800795,210.346893954693,1.00234807511964));
#11869=CARTESIAN_POINT('Ctrl Pts',(-7.45558679680064,210.281951283189,0.85081417035268));
#11870=CARTESIAN_POINT('Ctrl Pts',(-7.46978916139896,210.217273190525,0.699053789843961));
#11871=CARTESIAN_POINT('Ctrl Pts',(-7.48399533711949,210.152577741871,0.54725268531685));
#11872=CARTESIAN_POINT('Ctrl Pts',(-7.49355053594383,210.088147231022,0.395225509158903));
#11873=CARTESIAN_POINT('Ctrl Pts',(-7.49847882953766,210.02415727582,0.243395891140488));
#11874=CARTESIAN_POINT('Ctrl Pts',(-7.49904738356035,210.016775056041,0.225880023133914));
#11875=CARTESIAN_POINT('Ctrl Pts',(-7.49955441349819,210.009398692253,0.208366777074336));
#11876=CARTESIAN_POINT('Ctrl Pts',(-7.5,210.002028447915,0.190856796705278));
#11877=CARTESIAN_POINT('Ctrl Pts',(-7.50386255306115,209.938139708658,0.0390720635509829));
#11878=CARTESIAN_POINT('Ctrl Pts',(-7.50312239555638,209.87379055128,-0.11319341637498));
#11879=CARTESIAN_POINT('Ctrl Pts',(-7.49772806215971,209.809155844927,-0.265518780411782));
#11880=CARTESIAN_POINT('Ctrl Pts',(-7.49212716810081,209.74204613624,-0.423677011228724));
#11881=CARTESIAN_POINT('Ctrl Pts',(-7.48150838279936,209.674628800622,-0.581899244411169));
#11882=CARTESIAN_POINT('Ctrl Pts',(-7.46587290795738,209.607105531561,-0.739708076930746));
#11883=CARTESIAN_POINT('Ctrl Pts',(-7.4508160992348,209.542081286575,-0.891676432864672));
#11884=CARTESIAN_POINT('Ctrl Pts',(-7.43110741988636,209.476959054234,-1.04326087688651));
#11885=CARTESIAN_POINT('Ctrl Pts',(-7.40680096324212,209.411920847683,-1.19403760734917));
#11886=CARTESIAN_POINT('Ctrl Pts',(-7.38249873476809,209.346893954693,-1.34478810981454));
#11887=CARTESIAN_POINT('Ctrl Pts',(-7.35360044359533,209.281951283189,-1.49473066237887));
#11888=CARTESIAN_POINT('Ctrl Pts',(-7.32021115834334,209.217273190525,-1.64345213319835));
#11889=CARTESIAN_POINT('Ctrl Pts',(-7.28681291327022,209.152577741871,-1.79221351256238));
#11890=CARTESIAN_POINT('Ctrl Pts',(-7.24892146633696,209.088147231022,-1.93975266792269));
#11891=CARTESIAN_POINT('Ctrl Pts',(-7.20669061985644,209.02415727582,-2.08567414197946));
#11892=CARTESIAN_POINT('Ctrl Pts',(-7.20181864597934,209.016775056041,-2.10250841524085));
#11893=CARTESIAN_POINT('Ctrl Pts',(-7.19688896944662,209.009398692253,-2.11932118289467));
#11894=CARTESIAN_POINT('Ctrl Pts',(-7.19190186588755,209.002028447915,-2.13611185762632));
#11895=CARTESIAN_POINT('Ctrl Pts',(-7.14867131011455,208.938139708658,-2.28166131170439));
#11896=CARTESIAN_POINT('Ctrl Pts',(-7.10091475754278,208.87379055128,-2.42624566734729));
#11897=CARTESIAN_POINT('Ctrl Pts',(-7.0487133154531,208.809155844927,-2.56944875671861));
#11898=CARTESIAN_POINT('Ctrl Pts',(-6.99451296753859,208.74204613624,-2.71813540129489));
#11899=CARTESIAN_POINT('Ctrl Pts',(-6.93552054364117,208.674628800623,-2.86533230206806));
#11900=CARTESIAN_POINT('Ctrl Pts',(-6.87188471229632,208.607105531561,-3.01058579312345));
#11901=CARTESIAN_POINT('Ctrl Pts',(-6.8106040316553,208.542081286575,-3.15046347852873));
#11902=CARTESIAN_POINT('Ctrl Pts',(-6.74501779444778,208.476959054234,-3.28853853492931));
#11903=CARTESIAN_POINT('Ctrl Pts',(-6.67530840839898,208.411920847683,-3.42442461876539));
#11904=CARTESIAN_POINT('Ctrl Pts',(-6.60561114847592,208.346893954693,-3.56028706487013));
#11905=CARTESIAN_POINT('Ctrl Pts',(-6.53179244342397,208.281951283189,-3.69396084347553));
#11906=CARTESIAN_POINT('Ctrl Pts',(-6.45407988419901,208.217273190525,-3.82508551083845));
#11907=CARTESIAN_POINT('Ctrl Pts',(-6.37634647125933,208.152577741871,-3.95624536474565));
#11908=CARTESIAN_POINT('Ctrl Pts',(-6.29471745739962,208.088147231022,-4.08485433881581));
#11909=CARTESIAN_POINT('Ctrl Pts',(-6.20946132033797,208.02415727582,-4.21058385833547));
#11910=CARTESIAN_POINT('Ctrl Pts',(-6.19962572130909,208.016775056041,-4.22508868089382));
#11911=CARTESIAN_POINT('Ctrl Pts',(-6.18974188939178,208.009398692253,-4.23955521930275));
#11912=CARTESIAN_POINT('Ctrl Pts',(-6.17981026821526,208.002028447915,-4.253983000167));
#11913=CARTESIAN_POINT('Ctrl Pts',(-6.09371831161218,207.938139708658,-4.379049780501));
#11914=CARTESIAN_POINT('Ctrl Pts',(-6.00362010807862,207.87379055128,-4.50180008775205));
#11915=CARTESIAN_POINT('Ctrl Pts',(-5.90972139815651,207.809155844927,-4.62186318631563));
#11916=CARTESIAN_POINT('Ctrl Pts',(-5.81222710407629,207.74204613624,-4.74652375991935));
#11917=CARTESIAN_POINT('Ctrl Pts',(-5.71063563105837,207.674628800623,-4.86828667005446));
#11918=CARTESIAN_POINT('Ctrl Pts',(-5.60522856175958,207.607105531561,-4.98676639590057));
#11919=CARTESIAN_POINT('Ctrl Pts',(-5.50372258918887,207.542081286575,-5.10086120834461));
#11920=CARTESIAN_POINT('Ctrl Pts',(-5.39867883198632,207.476959054234,-5.21191112857799));
#11921=CARTESIAN_POINT('Ctrl Pts',(-5.29039015693326,207.411920847683,-5.3196050891276));
#11922=CARTESIAN_POINT('Ctrl Pts',(-5.18212031897177,207.346893954693,-5.42728031603775));
#11923=CARTESIAN_POINT('Ctrl Pts',(-5.07060708921622,207.281951283189,-5.53160039987444));
#11924=CARTESIAN_POINT('Ctrl Pts',(-4.95617830277041,207.217273190525,-5.63229286774013));
#11925=CARTESIAN_POINT('Ctrl Pts',(-4.8417188100227,207.152577741871,-5.73301235584621));
#11926=CARTESIAN_POINT('Ctrl Pts',(-4.72434264585535,207.088147231022,-5.83010200617336));
#11927=CARTESIAN_POINT('Ctrl Pts',(-4.60440668292199,207.024157275819,-5.92333228977675));
#11928=CARTESIAN_POINT('Ctrl Pts',(-4.59057023570353,207.016775056041,-5.93408782853836));
#11929=CARTESIAN_POINT('Ctrl Pts',(-4.57669974673502,207.009398692253,-5.94479205212799));
#11930=CARTESIAN_POINT('Ctrl Pts',(-4.56279578422009,207.002028447915,-5.95544464740895));
#11931=CARTESIAN_POINT('Ctrl Pts',(-4.44226970733713,206.938139708658,-6.04778634614835));
#11932=CARTESIAN_POINT('Ctrl Pts',(-4.31864929275468,206.87379055128,-6.1366869496822));
#11933=CARTESIAN_POINT('Ctrl Pts',(-4.19224477495804,206.809155844927,-6.22185744482189));
#11934=CARTESIAN_POINT('Ctrl Pts',(-4.06099995549939,206.74204613624,-6.31028930194741));
#11935=CARTESIAN_POINT('Ctrl Pts',(-3.92675391456938,206.674628800622,-6.39469921942834));
#11936=CARTESIAN_POINT('Ctrl Pts',(-3.78989358567387,206.607105531561,-6.47480755900256));
#11937=CARTESIAN_POINT('Ctrl Pts',(-3.65809843300235,206.542081286575,-6.55195110329805));
#11938=CARTESIAN_POINT('Ctrl Pts',(-3.52387957064261,206.476959054234,-6.62510554744148));
#11939=CARTESIAN_POINT('Ctrl Pts',(-3.38761165659103,206.411920847683,-6.69406554949809));
#11940=CARTESIAN_POINT('Ctrl Pts',(-3.25136744669109,206.346893954693,-6.76301355578624));
#11941=CARTESIAN_POINT('Ctrl Pts',(-3.11307538411878,206.281951283189,-6.82776836820748));
#11942=CARTESIAN_POINT('Ctrl Pts',(-2.97313145734166,206.217273190525,-6.88817215625554));
#11943=CARTESIAN_POINT('Ctrl Pts',(-2.8331499774231,206.152577741871,-6.94859215330993));
#11944=CARTESIAN_POINT('Ctrl Pts',(-2.69151625970553,206.088147231022,-7.00465866845592));
#11945=CARTESIAN_POINT('Ctrl Pts',(-2.54864063859631,206.02415727582,-7.05626368640968));
#11946=CARTESIAN_POINT('Ctrl Pts',(-2.53215775104539,206.016775056041,-7.06221711430306));
#11947=CARTESIAN_POINT('Ctrl Pts',(-2.51565834512647,206.009398692253,-7.06811121908845));
#11948=CARTESIAN_POINT('Ctrl Pts',(-2.49914305799788,206.002028447915,-7.07394587853976));
#11949=CARTESIAN_POINT('Ctrl Pts',(-2.35598079299498,205.938139708658,-7.12452344682942));
#11950=CARTESIAN_POINT('Ctrl Pts',(-2.21093899485714,205.87379055128,-7.1708721361652));
#11951=CARTESIAN_POINT('Ctrl Pts',(-2.06440202410006,205.809155844927,-7.21281294639894));
#11952=CARTESIAN_POINT('Ctrl Pts',(-1.91225383662799,205.74204613624,-7.25635976072986));
#11953=CARTESIAN_POINT('Ctrl Pts',(-1.75849416561927,205.674628800623,-7.29515405471511));
#11954=CARTESIAN_POINT('Ctrl Pts',(-1.60357741968129,205.607105531561,-7.32904944559231));
#11955=CARTESIAN_POINT('Ctrl Pts',(-1.45439411472333,205.542081286575,-7.36169037413289));
#11956=CARTESIAN_POINT('Ctrl Pts',(-1.30413842461202,205.476959054234,-7.38978847549662));
#11957=CARTESIAN_POINT('Ctrl Pts',(-1.15323012442371,205.411920847683,-7.41326423358633));
#11958=CARTESIAN_POINT('Ctrl Pts',(-1.00234807511963,205.346893954693,-7.43673590800795));
#11959=CARTESIAN_POINT('Ctrl Pts',(-0.850814170352673,205.281951283189,
-7.45558679680064));
#11960=CARTESIAN_POINT('Ctrl Pts',(-0.699053789843954,205.217273190525,
-7.46978916139896));
#11961=CARTESIAN_POINT('Ctrl Pts',(-0.547252685316885,205.152577741871,
-7.48399533711949));
#11962=CARTESIAN_POINT('Ctrl Pts',(-0.39522550915898,205.088147231022,-7.49355053594382));
#11963=CARTESIAN_POINT('Ctrl Pts',(-0.243395891140606,205.02415727582,-7.49847882953766));
#11964=CARTESIAN_POINT('Ctrl Pts',(-0.225880023133996,205.016775056041,
-7.49904738356035));
#11965=CARTESIAN_POINT('Ctrl Pts',(-0.208366777074381,205.009398692253,
-7.49955441349818));
#11966=CARTESIAN_POINT('Ctrl Pts',(-0.190856796705286,205.002028447915,
-7.5));
#11967=CARTESIAN_POINT('Ctrl Pts',(-0.0390720635510205,204.938139708658,
-7.50386255306115));
#11968=CARTESIAN_POINT('Ctrl Pts',(0.113193416374905,204.87379055128,-7.50312239555638));
#11969=CARTESIAN_POINT('Ctrl Pts',(0.265518780411678,204.809155844927,-7.49772806215972));
#11970=CARTESIAN_POINT('Ctrl Pts',(0.42367701122863,204.74204613624,-7.49212716810082));
#11971=CARTESIAN_POINT('Ctrl Pts',(0.581899244411101,204.674628800623,-7.48150838279936));
#11972=CARTESIAN_POINT('Ctrl Pts',(0.739708076930687,204.607105531561,-7.46587290795739));
#11973=CARTESIAN_POINT('Ctrl Pts',(0.891676432865158,204.542081286575,-7.45081609923475));
#11974=CARTESIAN_POINT('Ctrl Pts',(1.04326087688753,204.476959054234,-7.43110741988623));
#11975=CARTESIAN_POINT('Ctrl Pts',(1.19403760735073,204.411920847682,-7.40680096324187));
#11976=CARTESIAN_POINT('Ctrl Pts',(1.34478810981601,204.346893954693,-7.38249873476782));
#11977=CARTESIAN_POINT('Ctrl Pts',(1.49473066238024,204.281951283188,-7.35360044359504));
#11978=CARTESIAN_POINT('Ctrl Pts',(1.64345213319964,204.217273190525,-7.32021115834305));
#11979=CARTESIAN_POINT('Ctrl Pts',(1.79221351256366,204.15257774187,-7.28681291326991));
#11980=CARTESIAN_POINT('Ctrl Pts',(1.93975266792397,204.088147231022,-7.24892146633662));
#11981=CARTESIAN_POINT('Ctrl Pts',(2.08567414198074,204.024157275819,-7.20669061985607));
#11982=CARTESIAN_POINT('Ctrl Pts',(2.1025084152417,204.016775056041,-7.20181864597909));
#11983=CARTESIAN_POINT('Ctrl Pts',(2.1193211828951,204.009398692253,-7.19688896944649));
#11984=CARTESIAN_POINT('Ctrl Pts',(2.13611185762632,204.002028447915,-7.19190186588755));
#11985=CARTESIAN_POINT('Ctrl Pts',(2.28166131170441,203.938139708658,-7.14867131011454));
#11986=CARTESIAN_POINT('Ctrl Pts',(2.42624566734732,203.87379055128,-7.10091475754277));
#11987=CARTESIAN_POINT('Ctrl Pts',(2.56944875671865,203.809155844927,-7.04871331545308));
#11988=CARTESIAN_POINT('Ctrl Pts',(2.71813540129493,203.74204613624,-6.99451296753857));
#11989=CARTESIAN_POINT('Ctrl Pts',(2.86533230206809,203.674628800623,-6.93552054364115));
#11990=CARTESIAN_POINT('Ctrl Pts',(3.01058579312348,203.607105531561,-6.87188471229631));
#11991=CARTESIAN_POINT('Ctrl Pts',(3.15046347852877,203.542081286575,-6.81060403165528));
#11992=CARTESIAN_POINT('Ctrl Pts',(3.28853853492937,203.476959054234,-6.74501779444775));
#11993=CARTESIAN_POINT('Ctrl Pts',(3.42442461876546,203.411920847683,-6.67530840839894));
#11994=CARTESIAN_POINT('Ctrl Pts',(3.56028706487072,203.346893954693,-6.60561114847562));
#11995=CARTESIAN_POINT('Ctrl Pts',(3.69396084347661,203.281951283188,-6.53179244342338));
#11996=CARTESIAN_POINT('Ctrl Pts',(3.82508551084001,203.217273190525,-6.45407988419809));
#11997=CARTESIAN_POINT('Ctrl Pts',(3.95624536474729,203.15257774187,-6.37634647125832));
#11998=CARTESIAN_POINT('Ctrl Pts',(4.08485433881753,203.088147231021,-6.29471745739851));
#11999=CARTESIAN_POINT('Ctrl Pts',(4.21058385833727,203.024157275819,-6.20946132033675));
#12000=CARTESIAN_POINT('Ctrl Pts',(4.22508868089501,203.016775056041,-6.19962572130827));
#12001=CARTESIAN_POINT('Ctrl Pts',(4.23955521930334,203.009398692253,-6.18974188939137));
#12002=CARTESIAN_POINT('Ctrl Pts',(4.25398300016701,203.002028447915,-6.17981026821526));
#12003=CARTESIAN_POINT('Ctrl Pts',(4.37904978050104,202.938139708658,-6.09371831161216));
#12004=CARTESIAN_POINT('Ctrl Pts',(4.50180008775212,202.87379055128,-6.00362010807857));
#12005=CARTESIAN_POINT('Ctrl Pts',(4.62186318631574,202.809155844927,-5.90972139815643));
#12006=CARTESIAN_POINT('Ctrl Pts',(4.74652375991944,202.74204613624,-5.81222710407621));
#12007=CARTESIAN_POINT('Ctrl Pts',(4.86828667005455,202.674628800622,-5.71063563105829));
#12008=CARTESIAN_POINT('Ctrl Pts',(4.98676639590066,202.607105531561,-5.60522856175951));
#12009=CARTESIAN_POINT('Ctrl Pts',(5.10086120834481,202.542081286575,-5.50372258918869));
#12010=CARTESIAN_POINT('Ctrl Pts',(5.21191112857829,202.476959054234,-5.39867883198603));
#12011=CARTESIAN_POINT('Ctrl Pts',(5.319605089128,202.411920847683,-5.29039015693286));
#12012=CARTESIAN_POINT('Ctrl Pts',(5.42728031603811,202.346893954693,-5.1821203189714));
#12013=CARTESIAN_POINT('Ctrl Pts',(5.53160039987475,202.281951283188,-5.07060708921589));
#12014=CARTESIAN_POINT('Ctrl Pts',(5.6322928677404,202.217273190525,-4.95617830277011));
#12015=CARTESIAN_POINT('Ctrl Pts',(5.73301235584613,202.152577741871,-4.84171881002279));
#12016=CARTESIAN_POINT('Ctrl Pts',(5.83010200617296,202.088147231022,-4.72434264585582));
#12017=CARTESIAN_POINT('Ctrl Pts',(5.92333228977606,202.024157275819,-4.60440668292288));
#12018=CARTESIAN_POINT('Ctrl Pts',(5.93408782853791,202.016775056041,-4.59057023570412));
#12019=CARTESIAN_POINT('Ctrl Pts',(5.94479205212776,202.009398692253,-4.57669974673532));
#12020=CARTESIAN_POINT('Ctrl Pts',(5.95544464740895,202.002028447915,-4.56279578422009));
#12021=CARTESIAN_POINT('Ctrl Pts',(6.04778634614835,201.938139708658,-4.44226970733712));
#12022=CARTESIAN_POINT('Ctrl Pts',(6.13668694968221,201.87379055128,-4.31864929275467));
#12023=CARTESIAN_POINT('Ctrl Pts',(6.22185744482191,201.809155844927,-4.19224477495801));
#12024=CARTESIAN_POINT('Ctrl Pts',(6.31028930194743,201.74204613624,-4.06099995549936));
#12025=CARTESIAN_POINT('Ctrl Pts',(6.39469921942835,201.674628800622,-3.92675391456936));
#12026=CARTESIAN_POINT('Ctrl Pts',(6.47480755900257,201.607105531561,-3.78989358567385));
#12027=CARTESIAN_POINT('Ctrl Pts',(6.55195110329815,201.542081286575,-3.65809843300218));
#12028=CARTESIAN_POINT('Ctrl Pts',(6.62510554744167,201.476959054234,-3.52387957064226));
#12029=CARTESIAN_POINT('Ctrl Pts',(6.69406554949835,201.411920847682,-3.38761165659051));
#12030=CARTESIAN_POINT('Ctrl Pts',(6.76301355578675,201.346893954693,-3.25136744669006));
#12031=CARTESIAN_POINT('Ctrl Pts',(6.8277683682082,201.281951283188,-3.11307538411724));
#12032=CARTESIAN_POINT('Ctrl Pts',(6.88817215625643,201.217273190524,-2.97313145733959));
#12033=CARTESIAN_POINT('Ctrl Pts',(6.94859215331078,201.15257774187,-2.83314997742101));
#12034=CARTESIAN_POINT('Ctrl Pts',(7.00465866845674,201.088147231021,-2.69151625970341));
#12035=CARTESIAN_POINT('Ctrl Pts',(7.05626368641046,201.024157275819,-2.54864063859417));
#12036=CARTESIAN_POINT('Ctrl Pts',(7.06221711430357,201.016775056041,-2.53215775104397));
#12037=CARTESIAN_POINT('Ctrl Pts',(7.0681112190887,201.009398692253,-2.51565834512576));
#12038=CARTESIAN_POINT('Ctrl Pts',(7.07394587853975,201.002028447915,-2.49914305799789));
#12039=CARTESIAN_POINT('Ctrl Pts',(7.12452344682944,200.938139708658,-2.35598079299493));
#12040=CARTESIAN_POINT('Ctrl Pts',(7.17087213616524,200.87379055128,-2.21093899485702));
#12041=CARTESIAN_POINT('Ctrl Pts',(7.21281294639899,200.809155844927,-2.06440202409988));
#12042=CARTESIAN_POINT('Ctrl Pts',(7.25635976072991,200.74204613624,-1.91225383662782));
#12043=CARTESIAN_POINT('Ctrl Pts',(7.29515405471514,200.674628800622,-1.75849416561912));
#12044=CARTESIAN_POINT('Ctrl Pts',(7.32904944559233,200.607105531561,-1.60357741968116));
#12045=CARTESIAN_POINT('Ctrl Pts',(7.36169037413292,200.542081286575,-1.45439411472321));
#12046=CARTESIAN_POINT('Ctrl Pts',(7.38978847549664,200.476959054234,-1.30413842461191));
#12047=CARTESIAN_POINT('Ctrl Pts',(7.41326423358634,200.411920847683,-1.15323012442361));
#12048=CARTESIAN_POINT('Ctrl Pts',(7.43673590800806,200.346893954693,-1.00234807511895));
#12049=CARTESIAN_POINT('Ctrl Pts',(7.4555867968008,200.281951283188,-0.850814170351404));
#12050=CARTESIAN_POINT('Ctrl Pts',(7.46978916139914,200.217273190525,-0.699053789842093));
#12051=CARTESIAN_POINT('Ctrl Pts',(7.48399533711963,200.15257774187,-0.547252685315009));
#12052=CARTESIAN_POINT('Ctrl Pts',(7.49355053594392,200.088147231021,-0.395225509157083));
#12053=CARTESIAN_POINT('Ctrl Pts',(7.49847882953772,200.024157275819,-0.243395891138698));
#12054=CARTESIAN_POINT('Ctrl Pts',(7.49904738356038,200.016775056041,-0.225880023132722));
#12055=CARTESIAN_POINT('Ctrl Pts',(7.4995544134982,200.009398692253,-0.208366777073748));
#12056=CARTESIAN_POINT('Ctrl Pts',(7.5,200.002028447915,-0.190856796705287));
#12057=CARTESIAN_POINT('Ctrl Pts',(7.50386255306115,199.938139708658,-0.0390720635509912));
#12058=CARTESIAN_POINT('Ctrl Pts',(7.50312239555638,199.87379055128,0.113193416374972));
#12059=CARTESIAN_POINT('Ctrl Pts',(7.49772806215971,199.809155844927,0.265518780411775));
#12060=CARTESIAN_POINT('Ctrl Pts',(7.49212716810081,199.74204613624,0.423677011228717));
#12061=CARTESIAN_POINT('Ctrl Pts',(7.48150838279936,199.674628800623,0.581899244411163));
#12062=CARTESIAN_POINT('Ctrl Pts',(7.46587290795738,199.607105531561,0.73970807693074));
#12063=CARTESIAN_POINT('Ctrl Pts',(7.4508160992348,199.542081286575,0.891676432864664));
#12064=CARTESIAN_POINT('Ctrl Pts',(7.43110741988637,199.476959054234,1.04326087688649));
#12065=CARTESIAN_POINT('Ctrl Pts',(7.40680096324213,199.411920847683,1.19403760734915));
#12066=CARTESIAN_POINT('Ctrl Pts',(7.38249873476819,199.346893954694,1.34478810981391));
#12067=CARTESIAN_POINT('Ctrl Pts',(7.35360044359557,199.281951283189,1.49473066237762));
#12068=CARTESIAN_POINT('Ctrl Pts',(7.32021115834376,199.217273190526,1.64345213319651));
#12069=CARTESIAN_POINT('Ctrl Pts',(7.28681291327069,199.152577741872,1.79221351256049));
#12070=CARTESIAN_POINT('Ctrl Pts',(7.24892146633748,199.088147231023,1.93975266792075));
#12071=CARTESIAN_POINT('Ctrl Pts',(7.20669061985702,199.02415727582,2.08567414197748));
#12072=CARTESIAN_POINT('Ctrl Pts',(7.20181864597973,199.016775056042,2.10250841523952));
#12073=CARTESIAN_POINT('Ctrl Pts',(7.19688896944681,199.009398692254,2.11932118289401));
#12074=CARTESIAN_POINT('Ctrl Pts',(7.19190186588755,199.002028447915,2.13611185762632));
#12075=CARTESIAN_POINT('Ctrl Pts',(7.14867131011454,198.938139708658,2.28166131170442));
#12076=CARTESIAN_POINT('Ctrl Pts',(7.10091475754276,198.87379055128,2.42624566734735));
#12077=CARTESIAN_POINT('Ctrl Pts',(7.04871331545307,198.809155844927,2.56944875671869));
#12078=CARTESIAN_POINT('Ctrl Pts',(6.99451296753856,198.74204613624,2.71813540129497));
#12079=CARTESIAN_POINT('Ctrl Pts',(6.93552054364114,198.674628800622,2.86533230206812));
#12080=CARTESIAN_POINT('Ctrl Pts',(6.8718847122963,198.607105531561,3.0105857931235));
#12081=CARTESIAN_POINT('Ctrl Pts',(6.81060403165536,198.542081286575,3.1504634785286));
#12082=CARTESIAN_POINT('Ctrl Pts',(6.74501779444792,198.476959054234,3.288538534929));
#12083=CARTESIAN_POINT('Ctrl Pts',(6.67530840839923,198.411920847683,3.42442461876491));
#12084=CARTESIAN_POINT('Ctrl Pts',(6.60561114847646,198.346893954694,3.56028706486911));
#12085=CARTESIAN_POINT('Ctrl Pts',(6.53179244342483,198.281951283189,3.69396084347398));
#12086=CARTESIAN_POINT('Ctrl Pts',(6.45407988420023,198.217273190526,3.8250855108364));
#12087=CARTESIAN_POINT('Ctrl Pts',(6.37634647126055,198.152577741872,3.9562453647437));
#12088=CARTESIAN_POINT('Ctrl Pts',(6.29471745740083,198.088147231023,4.08485433881396));
#12089=CARTESIAN_POINT('Ctrl Pts',(6.20946132033916,198.024157275821,4.21058385833372));
#12090=CARTESIAN_POINT('Ctrl Pts',(6.19962572130989,198.016775056042,4.22508868089265));
#12091=CARTESIAN_POINT('Ctrl Pts',(6.18974188939218,198.009398692254,4.23955521930217));
#12092=CARTESIAN_POINT('Ctrl Pts',(6.17981026821526,198.002028447915,4.25398300016701));
#12093=CARTESIAN_POINT('Ctrl Pts',(6.09371831161217,197.938139708658,4.37904978050101));
#12094=CARTESIAN_POINT('Ctrl Pts',(6.0036201080786,197.87379055128,4.50180008775207));
#12095=CARTESIAN_POINT('Ctrl Pts',(5.90972139815648,197.809155844927,4.62186318631566));
#12096=CARTESIAN_POINT('Ctrl Pts',(5.81222710407627,197.74204613624,4.74652375991938));
#12097=CARTESIAN_POINT('Ctrl Pts',(5.71063563105834,197.674628800623,4.86828667005449));
#12098=CARTESIAN_POINT('Ctrl Pts',(5.60522856175956,197.607105531561,4.9867663959006));
#12099=CARTESIAN_POINT('Ctrl Pts',(5.50372258918911,197.542081286575,5.10086120834435));
#12100=CARTESIAN_POINT('Ctrl Pts',(5.39867883198685,197.476959054235,5.21191112857743));
#12101=CARTESIAN_POINT('Ctrl Pts',(5.29039015693409,197.411920847683,5.31960508912677));
#12102=CARTESIAN_POINT('Ctrl Pts',(5.18212031897387,197.346893954695,5.4272803160357));
#12103=CARTESIAN_POINT('Ctrl Pts',(5.07060708921967,197.281951283191,5.53160039987124));
#12104=CARTESIAN_POINT('Ctrl Pts',(4.95617830277527,197.217273190528,5.63229286773586));
#12105=CARTESIAN_POINT('Ctrl Pts',(4.84171881002731,197.152577741873,5.73301235584234));
#12106=CARTESIAN_POINT('Ctrl Pts',(4.72434264585968,197.088147231024,5.83010200616986));
#12107=CARTESIAN_POINT('Ctrl Pts',(4.60440668292603,197.024157275821,5.92333228977361));
#12108=CARTESIAN_POINT('Ctrl Pts',(4.59057023570623,197.016775056042,5.93408782853628));
#12109=CARTESIAN_POINT('Ctrl Pts',(4.57669974673637,197.009398692254,5.94479205212695));
#12110=CARTESIAN_POINT('Ctrl Pts',(4.56279578422009,197.002028447915,5.95544464740895));
#12111=CARTESIAN_POINT('Ctrl Pts',(4.44226970733712,196.938139708658,6.04778634614835));
#12112=CARTESIAN_POINT('Ctrl Pts',(4.31864929275467,196.87379055128,6.13668694968221));
#12113=CARTESIAN_POINT('Ctrl Pts',(4.19224477495802,196.809155844927,6.22185744482191));
#12114=CARTESIAN_POINT('Ctrl Pts',(4.06099995549936,196.74204613624,6.31028930194743));
#12115=CARTESIAN_POINT('Ctrl Pts',(3.92675391456935,196.674628800622,6.39469921942835));
#12116=CARTESIAN_POINT('Ctrl Pts',(3.78989358567384,196.607105531561,6.47480755900257));
#12117=CARTESIAN_POINT('Ctrl Pts',(3.6580984330025,196.542081286575,6.55195110329796));
#12118=CARTESIAN_POINT('Ctrl Pts',(3.52387957064293,196.476959054234,6.62510554744131));
#12119=CARTESIAN_POINT('Ctrl Pts',(3.38761165659153,196.411920847683,6.69406554949784));
#12120=CARTESIAN_POINT('Ctrl Pts',(3.25136744669109,196.346893954693,6.76301355578625));
#12121=CARTESIAN_POINT('Ctrl Pts',(3.11307538411827,196.281951283188,6.82776836820773));
#12122=CARTESIAN_POINT('Ctrl Pts',(2.97313145734063,196.217273190525,6.88817215625598));
#12123=CARTESIAN_POINT('Ctrl Pts',(2.83314997742163,196.15257774187,6.94859215331054));
#12124=CARTESIAN_POINT('Ctrl Pts',(2.69151625970362,196.088147231021,7.00465866845667));
#12125=CARTESIAN_POINT('Ctrl Pts',(2.54864063859395,196.024157275819,7.05626368641054));
#12126=CARTESIAN_POINT('Ctrl Pts',(2.53215775104383,196.016775056041,7.06221711430362));
#12127=CARTESIAN_POINT('Ctrl Pts',(2.51565834512569,196.009398692253,7.06811121908872));
#12128=CARTESIAN_POINT('Ctrl Pts',(2.49914305799789,196.002028447915,7.07394587853975));
#12129=CARTESIAN_POINT('Ctrl Pts',(2.35598079299495,195.938139708658,7.12452344682943));
#12130=CARTESIAN_POINT('Ctrl Pts',(2.21093899485708,195.87379055128,7.17087213616522));
#12131=CARTESIAN_POINT('Ctrl Pts',(2.06440202409996,195.809155844927,7.21281294639897));
#12132=CARTESIAN_POINT('Ctrl Pts',(1.9122538366279,195.74204613624,7.25635976072989));
#12133=CARTESIAN_POINT('Ctrl Pts',(1.75849416561919,195.674628800623,7.29515405471513));
#12134=CARTESIAN_POINT('Ctrl Pts',(1.60357741968122,195.607105531561,7.32904944559232));
#12135=CARTESIAN_POINT('Ctrl Pts',(1.4543941147231,195.542081286575,7.36169037413294));
#12136=CARTESIAN_POINT('Ctrl Pts',(1.30413842461163,195.476959054234,7.38978847549669));
#12137=CARTESIAN_POINT('Ctrl Pts',(1.15323012442317,195.411920847683,7.41326423358641));
#12138=CARTESIAN_POINT('Ctrl Pts',(1.00234807511844,195.346893954693,7.43673590800813));
#12139=CARTESIAN_POINT('Ctrl Pts',(0.850814170350841,195.281951283188,7.45558679680086));
#12140=CARTESIAN_POINT('Ctrl Pts',(0.69905378984147,195.217273190524,7.46978916139919));
#12141=CARTESIAN_POINT('Ctrl Pts',(0.547252685314392,195.15257774187,7.48399533711967));
#12142=CARTESIAN_POINT('Ctrl Pts',(0.395225509156497,195.088147231021,7.49355053594395));
#12143=CARTESIAN_POINT('Ctrl Pts',(0.243395891138119,195.024157275819,7.49847882953774));
#12144=CARTESIAN_POINT('Ctrl Pts',(0.225880023132343,195.016775056041,7.4990473835604));
#12145=CARTESIAN_POINT('Ctrl Pts',(0.208366777073546,195.009398692253,7.49955441349821));
#12146=CARTESIAN_POINT('Ctrl Pts',(0.190856796705285,195.002028447915,7.5));
#12147=CARTESIAN_POINT('Ctrl Pts',(0.127311648028404,194.975281229334,7.50161706980302));
#12148=CARTESIAN_POINT('Ctrl Pts',(0.0636823578853578,194.948453397593,
7.50242803155527));
#12149=CARTESIAN_POINT('Ctrl Pts',(-4.06843965232862E-7,194.921557632927,
7.50242802810186));
#12150=CARTESIAN_POINT('Origin',(0.,240.,0.));
#12151=CARTESIAN_POINT('Ctrl Pts',(5.38002895896315E-16,217.99585953923,
7.50000000439337));
#12152=CARTESIAN_POINT('Ctrl Pts',(-1.18775172812189,217.495912211348,7.50000000439337));
#12153=CARTESIAN_POINT('Ctrl Pts',(-2.317383311169,216.995967593475,7.13300320026677));
#12154=CARTESIAN_POINT('Ctrl Pts',(-3.44714003087638,216.495967593475,6.76596574150984));
#12155=CARTESIAN_POINT('Ctrl Pts',(-4.40818170865423,215.995967593475,6.06777834873578));
#12156=CARTESIAN_POINT('Ctrl Pts',(-5.36922338643209,215.495967593475,5.36959095596173));
#12157=CARTESIAN_POINT('Ctrl Pts',(-6.06747656688843,214.995967593475,4.40859707573286));
#12158=CARTESIAN_POINT('Ctrl Pts',(-6.76572974734476,214.495967593475,3.447603195504));
#12159=CARTESIAN_POINT('Ctrl Pts',(-7.13284454416054,213.995967593475,2.31787160445521));
#12160=CARTESIAN_POINT('Ctrl Pts',(-7.49995934097631,213.495967593475,1.18814001340642));
#12161=CARTESIAN_POINT('Ctrl Pts',(-7.5,212.995967593475,0.000256710972401669));
#12162=CARTESIAN_POINT('Ctrl Pts',(-7.50004065902369,212.495967593475,-1.18762659146162));
#12163=CARTESIAN_POINT('Ctrl Pts',(-7.13300320026677,211.995967593475,-2.317383311169));
#12164=CARTESIAN_POINT('Ctrl Pts',(-6.76596574150984,211.495967593475,-3.44714003087638));
#12165=CARTESIAN_POINT('Ctrl Pts',(-6.06777834873578,210.995967593475,-4.40818170865423));
#12166=CARTESIAN_POINT('Ctrl Pts',(-5.36959095596173,210.495967593475,-5.36922338643209));
#12167=CARTESIAN_POINT('Ctrl Pts',(-4.40859707573286,209.995967593475,-6.06747656688843));
#12168=CARTESIAN_POINT('Ctrl Pts',(-3.447603195504,209.495967593475,-6.76572974734476));
#12169=CARTESIAN_POINT('Ctrl Pts',(-2.31787160445521,208.995967593475,-7.13284454416054));
#12170=CARTESIAN_POINT('Ctrl Pts',(-1.18814001340642,208.495967593475,-7.49995934097631));
#12171=CARTESIAN_POINT('Ctrl Pts',(-0.000256710972402128,207.995967593475,
-7.5));
#12172=CARTESIAN_POINT('Ctrl Pts',(1.18762659146162,207.495967593475,-7.50004065902369));
#12173=CARTESIAN_POINT('Ctrl Pts',(2.317383311169,206.995967593475,-7.13300320026677));
#12174=CARTESIAN_POINT('Ctrl Pts',(3.44714003087638,206.495967593475,-6.76596574150984));
#12175=CARTESIAN_POINT('Ctrl Pts',(4.40818170865423,205.995967593475,-6.06777834873578));
#12176=CARTESIAN_POINT('Ctrl Pts',(5.36922338643209,205.495967593475,-5.36959095596173));
#12177=CARTESIAN_POINT('Ctrl Pts',(6.06747656688843,204.995967593475,-4.40859707573286));
#12178=CARTESIAN_POINT('Ctrl Pts',(6.76572974734476,204.495967593475,-3.447603195504));
#12179=CARTESIAN_POINT('Ctrl Pts',(7.13284454416054,203.995967593475,-2.31787160445521));
#12180=CARTESIAN_POINT('Ctrl Pts',(7.49995934097631,203.495967593475,-1.18814001340642));
#12181=CARTESIAN_POINT('Ctrl Pts',(7.5,202.995967593475,-0.000256710972402588));
#12182=CARTESIAN_POINT('Ctrl Pts',(7.50004065902369,202.495967593475,1.18762659146162));
#12183=CARTESIAN_POINT('Ctrl Pts',(7.13300320026677,201.995967593475,2.317383311169));
#12184=CARTESIAN_POINT('Ctrl Pts',(6.76596574150984,201.495967593475,3.44714003087638));
#12185=CARTESIAN_POINT('Ctrl Pts',(6.06777834873579,200.995967593475,4.40818170865423));
#12186=CARTESIAN_POINT('Ctrl Pts',(5.36959095596173,200.495967593475,5.36922338643209));
#12187=CARTESIAN_POINT('Ctrl Pts',(4.40859707573286,199.995967593475,6.06747656688843));
#12188=CARTESIAN_POINT('Ctrl Pts',(3.447603195504,199.495967593475,6.76572974734476));
#12189=CARTESIAN_POINT('Ctrl Pts',(2.31787160445521,198.995967593475,7.13284454416054));
#12190=CARTESIAN_POINT('Ctrl Pts',(1.18814001340643,198.495967593475,7.49995934097631));
#12191=CARTESIAN_POINT('Ctrl Pts',(0.00025671097240121,197.995967593475,
7.5));
#12192=CARTESIAN_POINT('Ctrl Pts',(0.000128355486237033,197.995913566499,
7.50000000439337));
#12193=CARTESIAN_POINT('Ctrl Pts',(5.38866871829646E-16,197.99585953923,
7.50000000439337));
#12194=CARTESIAN_POINT('Ctrl Pts',(-4.06843934450864E-7,234.921557632927,
7.50242802810186));
#12195=CARTESIAN_POINT('Ctrl Pts',(-0.152090385416014,234.857323985265,
7.50242801985428));
#12196=CARTESIAN_POINT('Ctrl Pts',(-0.304485788638578,234.792702491972,
7.49779895914527));
#12197=CARTESIAN_POINT('Ctrl Pts',(-0.456762644215501,234.72787053402,7.48851081348607));
#12198=CARTESIAN_POINT('Ctrl Pts',(-0.609070650331329,234.663025313709,
7.4792207677959));
#12199=CARTESIAN_POINT('Ctrl Pts',(-0.761259533138642,234.597969762788,
7.46526968655066));
#12200=CARTESIAN_POINT('Ctrl Pts',(-0.912902720439174,234.532885263597,
7.44667945730601));
#12201=CARTESIAN_POINT('Ctrl Pts',(-1.06450493068721,234.467818351553,7.42809425151684));
#12202=CARTESIAN_POINT('Ctrl Pts',(-1.2155612127989,234.402722732839,7.40487246128567));
#12203=CARTESIAN_POINT('Ctrl Pts',(-1.36565093134662,234.3377801784,7.3770877621566));
#12204=CARTESIAN_POINT('Ctrl Pts',(-1.51579830432564,234.272812677376,7.34929239000448));
#12205=CARTESIAN_POINT('Ctrl Pts',(-1.66497786162574,234.207998581557,7.31693074896052));
#12206=CARTESIAN_POINT('Ctrl Pts',(-1.81278187771317,234.143517028959,7.28012693437987));
#12207=CARTESIAN_POINT('Ctrl Pts',(-1.92135204017761,234.096151789321,7.25309251248725));
#12208=CARTESIAN_POINT('Ctrl Pts',(-2.02918025203209,234.04896593395,7.22366229239563));
#12209=CARTESIAN_POINT('Ctrl Pts',(-2.13611185762633,234.002028447915,7.19190186588755));
#12210=CARTESIAN_POINT('Ctrl Pts',(-2.28166131170441,233.938139708658,7.14867131011454));
#12211=CARTESIAN_POINT('Ctrl Pts',(-2.42624566734732,233.87379055128,7.10091475754277));
#12212=CARTESIAN_POINT('Ctrl Pts',(-2.56944875671866,233.809155844927,7.04871331545308));
#12213=CARTESIAN_POINT('Ctrl Pts',(-2.71813540129493,233.74204613624,6.99451296753857));
#12214=CARTESIAN_POINT('Ctrl Pts',(-2.8653323020681,233.674628800622,6.93552054364115));
#12215=CARTESIAN_POINT('Ctrl Pts',(-3.01058579312348,233.607105531561,6.8718847122963));
#12216=CARTESIAN_POINT('Ctrl Pts',(-3.15046347852879,233.542081286575,6.81060403165527));
#12217=CARTESIAN_POINT('Ctrl Pts',(-3.28853853492939,233.476959054234,6.74501779444774));
#12218=CARTESIAN_POINT('Ctrl Pts',(-3.42442461876549,233.411920847683,6.67530840839893));
#12219=CARTESIAN_POINT('Ctrl Pts',(-3.56028706487034,233.346893954693,6.60561114847581));
#12220=CARTESIAN_POINT('Ctrl Pts',(-3.69396084347583,233.281951283188,6.5317924434238));
#12221=CARTESIAN_POINT('Ctrl Pts',(-3.82508551083885,233.217273190525,6.45407988419878));
#12222=CARTESIAN_POINT('Ctrl Pts',(-3.95624536474616,233.152577741871,6.37634647125902));
#12223=CARTESIAN_POINT('Ctrl Pts',(-4.08485433881642,233.088147231022,6.29471745739923));
#12224=CARTESIAN_POINT('Ctrl Pts',(-4.21058385833618,233.024157275819,6.20946132033749));
#12225=CARTESIAN_POINT('Ctrl Pts',(-4.22508868089429,233.016775056041,6.19962572130877));
#12226=CARTESIAN_POINT('Ctrl Pts',(-4.23955521930298,233.009398692253,6.18974188939162));
#12227=CARTESIAN_POINT('Ctrl Pts',(-4.25398300016701,233.002028447915,6.17981026821526));
#12228=CARTESIAN_POINT('Ctrl Pts',(-4.3790497805011,232.938139708658,6.09371831161211));
#12229=CARTESIAN_POINT('Ctrl Pts',(-4.50180008775226,232.87379055128,6.00362010807847));
#12230=CARTESIAN_POINT('Ctrl Pts',(-4.62186318631593,232.809155844927,5.90972139815627));
#12231=CARTESIAN_POINT('Ctrl Pts',(-4.74652375991963,232.74204613624,5.81222710407607));
#12232=CARTESIAN_POINT('Ctrl Pts',(-4.86828667005471,232.674628800622,5.71063563105815));
#12233=CARTESIAN_POINT('Ctrl Pts',(-4.9867663959008,232.607105531561,5.60522856175938));
#12234=CARTESIAN_POINT('Ctrl Pts',(-5.10086120834483,232.542081286575,5.50372258918868));
#12235=CARTESIAN_POINT('Ctrl Pts',(-5.21191112857818,232.476959054234,5.39867883198613));
#12236=CARTESIAN_POINT('Ctrl Pts',(-5.31960508912778,232.411920847683,5.29039015693308));
#12237=CARTESIAN_POINT('Ctrl Pts',(-5.4272803160379,232.346893954693,5.18212031897162));
#12238=CARTESIAN_POINT('Ctrl Pts',(-5.53160039987455,232.281951283189,5.07060708921611));
#12239=CARTESIAN_POINT('Ctrl Pts',(-5.63229286774021,232.217273190525,4.95617830277033));
#12240=CARTESIAN_POINT('Ctrl Pts',(-5.7330123558459,232.152577741871,4.84171881002306));
#12241=CARTESIAN_POINT('Ctrl Pts',(-5.83010200617269,232.088147231022,4.72434264585615));
#12242=CARTESIAN_POINT('Ctrl Pts',(-5.92333228977576,232.02415727582,4.60440668292327));
#12243=CARTESIAN_POINT('Ctrl Pts',(-5.9340878285377,232.016775056041,4.59057023570438));
#12244=CARTESIAN_POINT('Ctrl Pts',(-5.94479205212766,232.009398692253,4.57669974673544));
#12245=CARTESIAN_POINT('Ctrl Pts',(-5.95544464740896,232.002028447915,4.56279578422008));
#12246=CARTESIAN_POINT('Ctrl Pts',(-6.04778634614836,231.938139708658,4.44226970733711));
#12247=CARTESIAN_POINT('Ctrl Pts',(-6.13668694968222,231.87379055128,4.31864929275465));
#12248=CARTESIAN_POINT('Ctrl Pts',(-6.22185744482192,231.809155844927,4.192244774958));
#12249=CARTESIAN_POINT('Ctrl Pts',(-6.31028930194744,231.74204613624,4.06099995549935));
#12250=CARTESIAN_POINT('Ctrl Pts',(-6.39469921942836,231.674628800622,3.92675391456934));
#12251=CARTESIAN_POINT('Ctrl Pts',(-6.47480755900258,231.607105531561,3.78989358567383));
#12252=CARTESIAN_POINT('Ctrl Pts',(-6.55195110329806,231.542081286575,3.65809843300233));
#12253=CARTESIAN_POINT('Ctrl Pts',(-6.62510554744149,231.476959054234,3.52387957064259));
#12254=CARTESIAN_POINT('Ctrl Pts',(-6.6940655494981,231.411920847683,3.38761165659102));
#12255=CARTESIAN_POINT('Ctrl Pts',(-6.76301355578627,231.346893954693,3.25136744669103));
#12256=CARTESIAN_POINT('Ctrl Pts',(-6.82776836820753,231.281951283188,3.11307538411867));
#12257=CARTESIAN_POINT('Ctrl Pts',(-6.8881721562556,231.217273190525,2.97313145734151));
#12258=CARTESIAN_POINT('Ctrl Pts',(-6.94859215330999,231.152577741871,2.83314997742295));
#12259=CARTESIAN_POINT('Ctrl Pts',(-7.00465866845598,231.088147231022,2.69151625970537));
#12260=CARTESIAN_POINT('Ctrl Pts',(-7.05626368640974,231.024157275819,2.54864063859615));
#12261=CARTESIAN_POINT('Ctrl Pts',(-7.06221711430309,231.016775056041,2.53215775104529));
#12262=CARTESIAN_POINT('Ctrl Pts',(-7.06811121908846,231.009398692253,2.51565834512643));
#12263=CARTESIAN_POINT('Ctrl Pts',(-7.07394587853975,231.002028447915,2.49914305799789));
#12264=CARTESIAN_POINT('Ctrl Pts',(-7.12452344682943,230.938139708658,2.35598079299495));
#12265=CARTESIAN_POINT('Ctrl Pts',(-7.17087213616522,230.87379055128,2.21093899485707));
#12266=CARTESIAN_POINT('Ctrl Pts',(-7.21281294639897,230.809155844927,2.06440202409995));
#12267=CARTESIAN_POINT('Ctrl Pts',(-7.25635976072989,230.74204613624,1.91225383662789));
#12268=CARTESIAN_POINT('Ctrl Pts',(-7.29515405471513,230.674628800623,1.75849416561917));
#12269=CARTESIAN_POINT('Ctrl Pts',(-7.32904944559233,230.607105531561,1.6035774196812));
#12270=CARTESIAN_POINT('Ctrl Pts',(-7.36169037413292,230.542081286575,1.45439411472321));
#12271=CARTESIAN_POINT('Ctrl Pts',(-7.38978847549665,230.476959054234,1.30413842461186));
#12272=CARTESIAN_POINT('Ctrl Pts',(-7.41326423358636,230.411920847683,1.15323012442351));
#12273=CARTESIAN_POINT('Ctrl Pts',(-7.43673590800799,230.346893954693,1.00234807511941));
#12274=CARTESIAN_POINT('Ctrl Pts',(-7.45558679680067,230.281951283188,0.850814170352427));
#12275=CARTESIAN_POINT('Ctrl Pts',(-7.46978916139899,230.217273190525,0.699053789843682));
#12276=CARTESIAN_POINT('Ctrl Pts',(-7.48399533711951,230.152577741871,0.547252685316623));
#12277=CARTESIAN_POINT('Ctrl Pts',(-7.49355053594384,230.088147231022,0.395225509158728));
#12278=CARTESIAN_POINT('Ctrl Pts',(-7.49847882953767,230.02415727582,0.243395891140365));
#12279=CARTESIAN_POINT('Ctrl Pts',(-7.49904738356035,230.016775056041,0.225880023133833));
#12280=CARTESIAN_POINT('Ctrl Pts',(-7.49955441349819,230.009398692253,0.208366777074296));
#12281=CARTESIAN_POINT('Ctrl Pts',(-7.5,230.002028447915,0.19085679670528));
#12282=CARTESIAN_POINT('Ctrl Pts',(-7.50386255306115,229.938139708658,0.0390720635509798));
#12283=CARTESIAN_POINT('Ctrl Pts',(-7.50312239555638,229.87379055128,-0.113193416374988));
#12284=CARTESIAN_POINT('Ctrl Pts',(-7.49772806215971,229.809155844927,-0.265518780411795));
#12285=CARTESIAN_POINT('Ctrl Pts',(-7.49212716810081,229.74204613624,-0.423677011228737));
#12286=CARTESIAN_POINT('Ctrl Pts',(-7.48150838279935,229.674628800622,-0.581899244411182));
#12287=CARTESIAN_POINT('Ctrl Pts',(-7.46587290795738,229.607105531561,-0.739708076930759));
#12288=CARTESIAN_POINT('Ctrl Pts',(-7.4508160992348,229.542081286575,-0.891676432864674));
#12289=CARTESIAN_POINT('Ctrl Pts',(-7.43110741988637,229.476959054234,-1.0432608768865));
#12290=CARTESIAN_POINT('Ctrl Pts',(-7.40680096324213,229.411920847683,-1.19403760734915));
#12291=CARTESIAN_POINT('Ctrl Pts',(-7.38249873476809,229.346893954693,-1.34478810981454));
#12292=CARTESIAN_POINT('Ctrl Pts',(-7.35360044359533,229.281951283189,-1.49473066237887));
#12293=CARTESIAN_POINT('Ctrl Pts',(-7.32021115834334,229.217273190525,-1.64345213319836));
#12294=CARTESIAN_POINT('Ctrl Pts',(-7.28681291327022,229.152577741871,-1.79221351256241));
#12295=CARTESIAN_POINT('Ctrl Pts',(-7.24892146633694,229.088147231022,-1.93975266792275));
#12296=CARTESIAN_POINT('Ctrl Pts',(-7.20669061985642,229.02415727582,-2.08567414197955));
#12297=CARTESIAN_POINT('Ctrl Pts',(-7.20181864597933,229.016775056041,-2.1025084152409));
#12298=CARTESIAN_POINT('Ctrl Pts',(-7.19688896944661,229.009398692253,-2.1193211828947));
#12299=CARTESIAN_POINT('Ctrl Pts',(-7.19190186588755,229.002028447915,-2.13611185762632));
#12300=CARTESIAN_POINT('Ctrl Pts',(-7.14867131011454,228.938139708658,-2.28166131170441));
#12301=CARTESIAN_POINT('Ctrl Pts',(-7.10091475754277,228.87379055128,-2.42624566734733));
#12302=CARTESIAN_POINT('Ctrl Pts',(-7.04871331545307,228.809155844927,-2.56944875671868));
#12303=CARTESIAN_POINT('Ctrl Pts',(-6.99451296753857,228.74204613624,-2.71813540129495));
#12304=CARTESIAN_POINT('Ctrl Pts',(-6.93552054364114,228.674628800622,-2.86533230206812));
#12305=CARTESIAN_POINT('Ctrl Pts',(-6.8718847122963,228.607105531561,-3.0105857931235));
#12306=CARTESIAN_POINT('Ctrl Pts',(-6.81060403165529,228.542081286575,-3.15046347852874));
#12307=CARTESIAN_POINT('Ctrl Pts',(-6.74501779444778,228.476959054234,-3.2885385349293));
#12308=CARTESIAN_POINT('Ctrl Pts',(-6.675308408399,228.411920847683,-3.42442461876534));
#12309=CARTESIAN_POINT('Ctrl Pts',(-6.60561114847594,228.346893954693,-3.5602870648701));
#12310=CARTESIAN_POINT('Ctrl Pts',(-6.53179244342398,228.281951283189,-3.69396084347551));
#12311=CARTESIAN_POINT('Ctrl Pts',(-6.45407988419902,228.217273190525,-3.82508551083845));
#12312=CARTESIAN_POINT('Ctrl Pts',(-6.37634647125928,228.152577741871,-3.95624536474574));
#12313=CARTESIAN_POINT('Ctrl Pts',(-6.29471745739952,228.088147231022,-4.08485433881598));
#12314=CARTESIAN_POINT('Ctrl Pts',(-6.2094613203378,228.02415727582,-4.21058385833573));
#12315=CARTESIAN_POINT('Ctrl Pts',(-6.19962572130897,228.016775056041,-4.22508868089399));
#12316=CARTESIAN_POINT('Ctrl Pts',(-6.18974188939172,228.009398692253,-4.23955521930283));
#12317=CARTESIAN_POINT('Ctrl Pts',(-6.17981026821526,228.002028447915,-4.25398300016701));
#12318=CARTESIAN_POINT('Ctrl Pts',(-6.09371831161215,227.938139708658,-4.37904978050104));
#12319=CARTESIAN_POINT('Ctrl Pts',(-6.00362010807856,227.87379055128,-4.50180008775213));
#12320=CARTESIAN_POINT('Ctrl Pts',(-5.90972139815641,227.809155844927,-4.62186318631575));
#12321=CARTESIAN_POINT('Ctrl Pts',(-5.8122271040762,227.74204613624,-4.74652375991946));
#12322=CARTESIAN_POINT('Ctrl Pts',(-5.71063563105828,227.674628800622,-4.86828667005456));
#12323=CARTESIAN_POINT('Ctrl Pts',(-5.6052285617595,227.607105531561,-4.98676639590066));
#12324=CARTESIAN_POINT('Ctrl Pts',(-5.50372258918886,227.542081286575,-5.10086120834462));
#12325=CARTESIAN_POINT('Ctrl Pts',(-5.39867883198638,227.476959054234,-5.21191112857791));
#12326=CARTESIAN_POINT('Ctrl Pts',(-5.29039015693341,227.411920847683,-5.31960508912745));
#12327=CARTESIAN_POINT('Ctrl Pts',(-5.18212031897197,227.346893954694,-5.42728031603756));
#12328=CARTESIAN_POINT('Ctrl Pts',(-5.07060708921648,227.281951283189,-5.5316003998742));
#12329=CARTESIAN_POINT('Ctrl Pts',(-4.95617830277073,227.217273190526,-5.63229286773986));
#12330=CARTESIAN_POINT('Ctrl Pts',(-4.84171881002346,227.152577741871,-5.73301235584555));
#12331=CARTESIAN_POINT('Ctrl Pts',(-4.72434264585657,227.088147231022,-5.83010200617235));
#12332=CARTESIAN_POINT('Ctrl Pts',(-4.60440668292369,227.02415727582,-5.92333228977543));
#12333=CARTESIAN_POINT('Ctrl Pts',(-4.59057023570467,227.016775056041,-5.93408782853748));
#12334=CARTESIAN_POINT('Ctrl Pts',(-4.57669974673559,227.009398692253,-5.94479205212755));
#12335=CARTESIAN_POINT('Ctrl Pts',(-4.56279578422009,227.002028447915,-5.95544464740895));
#12336=CARTESIAN_POINT('Ctrl Pts',(-4.44226970733717,226.938139708658,-6.04778634614832));
#12337=CARTESIAN_POINT('Ctrl Pts',(-4.31864929275475,226.87379055128,-6.13668694968215));
#12338=CARTESIAN_POINT('Ctrl Pts',(-4.19224477495815,226.809155844927,-6.22185744482182));
#12339=CARTESIAN_POINT('Ctrl Pts',(-4.06099995549949,226.74204613624,-6.31028930194735));
#12340=CARTESIAN_POINT('Ctrl Pts',(-3.92675391456947,226.674628800623,-6.39469921942828));
#12341=CARTESIAN_POINT('Ctrl Pts',(-3.78989358567395,226.607105531561,-6.47480755900251));
#12342=CARTESIAN_POINT('Ctrl Pts',(-3.65809843300246,226.542081286575,-6.55195110329799));
#12343=CARTESIAN_POINT('Ctrl Pts',(-3.52387957064274,226.476959054234,-6.62510554744141));
#12344=CARTESIAN_POINT('Ctrl Pts',(-3.38761165659118,226.411920847683,-6.69406554949802));
#12345=CARTESIAN_POINT('Ctrl Pts',(-3.25136744669125,226.346893954693,-6.76301355578616));
#12346=CARTESIAN_POINT('Ctrl Pts',(-3.11307538411895,226.281951283189,-6.8277683682074));
#12347=CARTESIAN_POINT('Ctrl Pts',(-2.97313145734185,226.217273190525,-6.88817215625545));
#12348=CARTESIAN_POINT('Ctrl Pts',(-2.83314997742316,226.152577741871,-6.94859215330991));
#12349=CARTESIAN_POINT('Ctrl Pts',(-2.69151625970544,226.088147231022,-7.00465866845596));
#12350=CARTESIAN_POINT('Ctrl Pts',(-2.54864063859608,226.024157275819,-7.05626368640977));
#12351=CARTESIAN_POINT('Ctrl Pts',(-2.53215775104524,226.016775056041,-7.06221711430311));
#12352=CARTESIAN_POINT('Ctrl Pts',(-2.5156583451264,226.009398692253,-7.06811121908847));
#12353=CARTESIAN_POINT('Ctrl Pts',(-2.49914305799788,226.002028447915,-7.07394587853975));
#12354=CARTESIAN_POINT('Ctrl Pts',(-2.35598079299495,225.938139708658,-7.12452344682943));
#12355=CARTESIAN_POINT('Ctrl Pts',(-2.21093899485708,225.87379055128,-7.17087213616522));
#12356=CARTESIAN_POINT('Ctrl Pts',(-2.06440202409996,225.809155844927,-7.21281294639897));
#12357=CARTESIAN_POINT('Ctrl Pts',(-1.9122538366279,225.74204613624,-7.25635976072989));
#12358=CARTESIAN_POINT('Ctrl Pts',(-1.75849416561919,225.674628800623,-7.29515405471513));
#12359=CARTESIAN_POINT('Ctrl Pts',(-1.60357741968122,225.607105531561,-7.32904944559232));
#12360=CARTESIAN_POINT('Ctrl Pts',(-1.45439411472326,225.542081286575,-7.36169037413291));
#12361=CARTESIAN_POINT('Ctrl Pts',(-1.30413842461196,225.476959054234,-7.38978847549663));
#12362=CARTESIAN_POINT('Ctrl Pts',(-1.15323012442366,225.411920847683,-7.41326423358633));
#12363=CARTESIAN_POINT('Ctrl Pts',(-1.00234807511957,225.346893954693,-7.43673590800797));
#12364=CARTESIAN_POINT('Ctrl Pts',(-0.850814170352588,225.281951283189,
-7.45558679680065));
#12365=CARTESIAN_POINT('Ctrl Pts',(-0.699053789843849,225.217273190525,
-7.46978916139897));
#12366=CARTESIAN_POINT('Ctrl Pts',(-0.547252685316753,225.152577741871,
-7.4839953371195));
#12367=CARTESIAN_POINT('Ctrl Pts',(-0.395225509158822,225.088147231022,
-7.49355053594383));
#12368=CARTESIAN_POINT('Ctrl Pts',(-0.243395891140422,225.02415727582,-7.49847882953767));
#12369=CARTESIAN_POINT('Ctrl Pts',(-0.225880023133874,225.016775056041,
-7.49904738356035));
#12370=CARTESIAN_POINT('Ctrl Pts',(-0.208366777074322,225.009398692253,
-7.49955441349819));
#12371=CARTESIAN_POINT('Ctrl Pts',(-0.19085679670529,225.002028447915,-7.5));
#12372=CARTESIAN_POINT('Ctrl Pts',(-0.0390720635510056,224.938139708658,
-7.50386255306115));
#12373=CARTESIAN_POINT('Ctrl Pts',(0.113193416374946,224.87379055128,-7.50312239555638));
#12374=CARTESIAN_POINT('Ctrl Pts',(0.265518780411738,224.809155844927,-7.49772806215971));
#12375=CARTESIAN_POINT('Ctrl Pts',(0.423677011228685,224.74204613624,-7.49212716810082));
#12376=CARTESIAN_POINT('Ctrl Pts',(0.581899244411136,224.674628800623,-7.48150838279936));
#12377=CARTESIAN_POINT('Ctrl Pts',(0.739708076930718,224.607105531561,-7.46587290795738));
#12378=CARTESIAN_POINT('Ctrl Pts',(0.891676432864649,224.542081286575,-7.4508160992348));
#12379=CARTESIAN_POINT('Ctrl Pts',(1.04326087688649,224.476959054234,-7.43110741988637));
#12380=CARTESIAN_POINT('Ctrl Pts',(1.19403760734915,224.411920847683,-7.40680096324213));
#12381=CARTESIAN_POINT('Ctrl Pts',(1.34478810981431,224.346893954693,-7.38249873476812));
#12382=CARTESIAN_POINT('Ctrl Pts',(1.49473066237841,224.281951283189,-7.35360044359541));
#12383=CARTESIAN_POINT('Ctrl Pts',(1.64345213319768,224.217273190526,-7.32021115834349));
#12384=CARTESIAN_POINT('Ctrl Pts',(1.79221351256174,224.152577741871,-7.28681291327038));
#12385=CARTESIAN_POINT('Ctrl Pts',(1.93975266792208,224.088147231022,-7.24892146633712));
#12386=CARTESIAN_POINT('Ctrl Pts',(2.08567414197888,224.02415727582,-7.20669061985661));
#12387=CARTESIAN_POINT('Ctrl Pts',(2.10250841524046,224.016775056041,-7.20181864597946));
#12388=CARTESIAN_POINT('Ctrl Pts',(2.11932118289448,224.009398692253,-7.19688896944667));
#12389=CARTESIAN_POINT('Ctrl Pts',(2.13611185762633,224.002028447915,-7.19190186588755));
#12390=CARTESIAN_POINT('Ctrl Pts',(2.28166131170461,223.938139708658,-7.14867131011448));
#12391=CARTESIAN_POINT('Ctrl Pts',(2.42624566734772,223.87379055128,-7.10091475754264));
#12392=CARTESIAN_POINT('Ctrl Pts',(2.56944875671925,223.809155844927,-7.04871331545287));
#12393=CARTESIAN_POINT('Ctrl Pts',(2.71813540129546,223.74204613624,-6.99451296753837));
#12394=CARTESIAN_POINT('Ctrl Pts',(2.86533230206858,223.674628800622,-6.93552054364095));
#12395=CARTESIAN_POINT('Ctrl Pts',(3.01058579312391,223.60710553156,-6.87188471229612));
#12396=CARTESIAN_POINT('Ctrl Pts',(3.1504634785292,223.542081286575,-6.81060403165508));
#12397=CARTESIAN_POINT('Ctrl Pts',(3.2885385349298,223.476959054234,-6.74501779444754));
#12398=CARTESIAN_POINT('Ctrl Pts',(3.42442461876589,223.411920847683,-6.67530840839872));
#12399=CARTESIAN_POINT('Ctrl Pts',(3.56028706487057,223.346893954693,-6.60561114847569));
#12400=CARTESIAN_POINT('Ctrl Pts',(3.69396084347589,223.281951283188,-6.53179244342376));
#12401=CARTESIAN_POINT('Ctrl Pts',(3.82508551083875,223.217273190525,-6.45407988419884));
#12402=CARTESIAN_POINT('Ctrl Pts',(3.95624536474612,223.152577741871,-6.37634647125905));
#12403=CARTESIAN_POINT('Ctrl Pts',(4.08485433881643,223.088147231022,-6.29471745739922));
#12404=CARTESIAN_POINT('Ctrl Pts',(4.21058385833625,223.024157275819,-6.20946132033745));
#12405=CARTESIAN_POINT('Ctrl Pts',(4.22508868089433,223.016775056041,-6.19962572130874));
#12406=CARTESIAN_POINT('Ctrl Pts',(4.239555219303,223.009398692253,-6.1897418893916));
#12407=CARTESIAN_POINT('Ctrl Pts',(4.253983000167,223.002028447915,-6.17981026821526));
#12408=CARTESIAN_POINT('Ctrl Pts',(4.379049780501,222.938139708658,-6.09371831161218));
#12409=CARTESIAN_POINT('Ctrl Pts',(4.50180008775205,222.87379055128,-6.00362010807862));
#12410=CARTESIAN_POINT('Ctrl Pts',(4.62186318631563,222.809155844927,-5.90972139815651));
#12411=CARTESIAN_POINT('Ctrl Pts',(4.74652375991935,222.74204613624,-5.81222710407629));
#12412=CARTESIAN_POINT('Ctrl Pts',(4.86828667005446,222.674628800623,-5.71063563105837));
#12413=CARTESIAN_POINT('Ctrl Pts',(4.98676639590057,222.607105531561,-5.60522856175958));
#12414=CARTESIAN_POINT('Ctrl Pts',(5.10086120834461,222.542081286575,-5.50372258918887));
#12415=CARTESIAN_POINT('Ctrl Pts',(5.21191112857799,222.476959054234,-5.39867883198631));
#12416=CARTESIAN_POINT('Ctrl Pts',(5.3196050891276,222.411920847683,-5.29039015693326));
#12417=CARTESIAN_POINT('Ctrl Pts',(5.42728031603795,222.346893954693,-5.18212031897158));
#12418=CARTESIAN_POINT('Ctrl Pts',(5.53160039987481,222.281951283188,-5.07060708921584));
#12419=CARTESIAN_POINT('Ctrl Pts',(5.63229286774066,222.217273190525,-4.95617830276981));
#12420=CARTESIAN_POINT('Ctrl Pts',(5.73301235584641,222.152577741871,-4.84171881002245));
#12421=CARTESIAN_POINT('Ctrl Pts',(5.83010200617326,222.088147231022,-4.72434264585545));
#12422=CARTESIAN_POINT('Ctrl Pts',(5.92333228977638,222.024157275819,-4.60440668292247));
#12423=CARTESIAN_POINT('Ctrl Pts',(5.93408782853811,222.016775056041,-4.59057023570385));
#12424=CARTESIAN_POINT('Ctrl Pts',(5.94479205212787,222.009398692253,-4.57669974673517));
#12425=CARTESIAN_POINT('Ctrl Pts',(5.95544464740896,222.002028447915,-4.56279578422009));
#12426=CARTESIAN_POINT('Ctrl Pts',(6.04778634614835,221.938139708658,-4.44226970733712));
#12427=CARTESIAN_POINT('Ctrl Pts',(6.13668694968221,221.87379055128,-4.31864929275467));
#12428=CARTESIAN_POINT('Ctrl Pts',(6.2218574448219,221.809155844927,-4.19224477495803));
#12429=CARTESIAN_POINT('Ctrl Pts',(6.31028930194743,221.74204613624,-4.06099995549937));
#12430=CARTESIAN_POINT('Ctrl Pts',(6.39469921942835,221.674628800622,-3.92675391456936));
#12431=CARTESIAN_POINT('Ctrl Pts',(6.47480755900257,221.607105531561,-3.78989358567385));
#12432=CARTESIAN_POINT('Ctrl Pts',(6.55195110329805,221.542081286575,-3.65809843300234));
#12433=CARTESIAN_POINT('Ctrl Pts',(6.62510554744149,221.476959054234,-3.5238795706426));
#12434=CARTESIAN_POINT('Ctrl Pts',(6.6940655494981,221.411920847683,-3.38761165659102));
#12435=CARTESIAN_POINT('Ctrl Pts',(6.76301355578647,221.346893954693,-3.25136744669064));
#12436=CARTESIAN_POINT('Ctrl Pts',(6.8277683682079,221.281951283188,-3.11307538411788));
#12437=CARTESIAN_POINT('Ctrl Pts',(6.88817215625612,221.217273190525,-2.9731314573403));
#12438=CARTESIAN_POINT('Ctrl Pts',(6.94859215331057,221.15257774187,-2.83314997742154));
#12439=CARTESIAN_POINT('Ctrl Pts',(7.00465866845661,221.088147231021,-2.69151625970376));
#12440=CARTESIAN_POINT('Ctrl Pts',(7.0562636864104,221.024157275819,-2.54864063859434));
#12441=CARTESIAN_POINT('Ctrl Pts',(7.06221711430353,221.016775056041,-2.53215775104408));
#12442=CARTESIAN_POINT('Ctrl Pts',(7.06811121908868,221.009398692253,-2.51565834512583));
#12443=CARTESIAN_POINT('Ctrl Pts',(7.07394587853975,221.002028447915,-2.4991430579979));
#12444=CARTESIAN_POINT('Ctrl Pts',(7.12452344682937,220.938139708658,-2.35598079299513));
#12445=CARTESIAN_POINT('Ctrl Pts',(7.17087213616511,220.87379055128,-2.21093899485743));
#12446=CARTESIAN_POINT('Ctrl Pts',(7.21281294639882,220.809155844927,-2.06440202410049));
#12447=CARTESIAN_POINT('Ctrl Pts',(7.25635976072976,220.74204613624,-1.91225383662838));
#12448=CARTESIAN_POINT('Ctrl Pts',(7.29515405471502,220.674628800623,-1.75849416561964));
#12449=CARTESIAN_POINT('Ctrl Pts',(7.32904944559223,220.607105531561,-1.60357741968163));
#12450=CARTESIAN_POINT('Ctrl Pts',(7.36169037413284,220.542081286575,-1.4543941147236));
#12451=CARTESIAN_POINT('Ctrl Pts',(7.38978847549659,220.476959054234,-1.30413842461222));
#12452=CARTESIAN_POINT('Ctrl Pts',(7.41326423358631,220.411920847683,-1.15323012442383));
#12453=CARTESIAN_POINT('Ctrl Pts',(7.43673590800786,220.346893954694,-1.00234807512029));
#12454=CARTESIAN_POINT('Ctrl Pts',(7.4555867968005,220.281951283189,-0.850814170353856));
#12455=CARTESIAN_POINT('Ctrl Pts',(7.4697891613988,220.217273190526,-0.69905378984567));
#12456=CARTESIAN_POINT('Ctrl Pts',(7.48399533711939,220.152577741872,-0.547252685318368));
#12457=CARTESIAN_POINT('Ctrl Pts',(7.49355053594376,220.088147231023,-0.395225509160228));
#12458=CARTESIAN_POINT('Ctrl Pts',(7.49847882953763,220.02415727582,-0.243395891141619));
#12459=CARTESIAN_POINT('Ctrl Pts',(7.49904738356033,220.016775056042,-0.22588002313467));
#12460=CARTESIAN_POINT('Ctrl Pts',(7.49955441349818,220.009398692253,-0.20836677707472));
#12461=CARTESIAN_POINT('Ctrl Pts',(7.5,220.002028447915,-0.190856796705287));
#12462=CARTESIAN_POINT('Ctrl Pts',(7.50386255306115,219.938139708658,-0.0390720635509813));
#12463=CARTESIAN_POINT('Ctrl Pts',(7.50312239555638,219.87379055128,0.113193416374992));
#12464=CARTESIAN_POINT('Ctrl Pts',(7.49772806215971,219.809155844927,0.265518780411804));
#12465=CARTESIAN_POINT('Ctrl Pts',(7.49212716810081,219.74204613624,0.423677011228746));
#12466=CARTESIAN_POINT('Ctrl Pts',(7.48150838279935,219.674628800622,0.581899244411192));
#12467=CARTESIAN_POINT('Ctrl Pts',(7.46587290795738,219.607105531561,0.739708076930769));
#12468=CARTESIAN_POINT('Ctrl Pts',(7.45081609923482,219.542081286575,0.891676432864501));
#12469=CARTESIAN_POINT('Ctrl Pts',(7.43110741988641,219.476959054234,1.04326087688616));
#12470=CARTESIAN_POINT('Ctrl Pts',(7.40680096324221,219.411920847683,1.19403760734863));
#12471=CARTESIAN_POINT('Ctrl Pts',(7.38249873476801,219.346893954693,1.34478810981507));
#12472=CARTESIAN_POINT('Ctrl Pts',(7.35360044359503,219.281951283188,1.49473066238045));
#12473=CARTESIAN_POINT('Ctrl Pts',(7.32021115834276,219.217273190524,1.64345213320097));
#12474=CARTESIAN_POINT('Ctrl Pts',(7.28681291326939,219.152577741869,1.79221351256585));
#12475=CARTESIAN_POINT('Ctrl Pts',(7.24892146633583,219.08814723102,1.93975266792699));
#12476=CARTESIAN_POINT('Ctrl Pts',(7.20669061985496,219.024157275817,2.08567414198458));
#12477=CARTESIAN_POINT('Ctrl Pts',(7.20181864597834,219.01677505604,2.10250841524425));
#12478=CARTESIAN_POINT('Ctrl Pts',(7.19688896944612,219.009398692252,2.11932118289636));
#12479=CARTESIAN_POINT('Ctrl Pts',(7.19190186588756,219.002028447915,2.13611185762631));
#12480=CARTESIAN_POINT('Ctrl Pts',(7.14867131011454,218.938139708658,2.28166131170442));
#12481=CARTESIAN_POINT('Ctrl Pts',(7.10091475754276,218.87379055128,2.42624566734735));
#12482=CARTESIAN_POINT('Ctrl Pts',(7.04871331545306,218.809155844927,2.56944875671871));
#12483=CARTESIAN_POINT('Ctrl Pts',(6.99451296753855,218.74204613624,2.71813540129498));
#12484=CARTESIAN_POINT('Ctrl Pts',(6.93552054364113,218.674628800622,2.86533230206815));
#12485=CARTESIAN_POINT('Ctrl Pts',(6.87188471229629,218.607105531561,3.01058579312352));
#12486=CARTESIAN_POINT('Ctrl Pts',(6.81060403165534,218.542081286575,3.15046347852863));
#12487=CARTESIAN_POINT('Ctrl Pts',(6.7450177944479,218.476959054234,3.28853853492905));
#12488=CARTESIAN_POINT('Ctrl Pts',(6.6753084083992,218.411920847683,3.42442461876496));
#12489=CARTESIAN_POINT('Ctrl Pts',(6.60561114847611,218.346893954694,3.56028706486978));
#12490=CARTESIAN_POINT('Ctrl Pts',(6.53179244342414,218.281951283189,3.69396084347523));
#12491=CARTESIAN_POINT('Ctrl Pts',(6.45407988419915,218.217273190526,3.82508551083821));
#12492=CARTESIAN_POINT('Ctrl Pts',(6.3763464712596,218.152577741871,3.95624536474522));
#12493=CARTESIAN_POINT('Ctrl Pts',(6.29471745740002,218.088147231023,4.0848543388152));
#12494=CARTESIAN_POINT('Ctrl Pts',(6.20946132033851,218.02415727582,4.21058385833468));
#12495=CARTESIAN_POINT('Ctrl Pts',(6.19962572130945,218.016775056042,4.22508868089329));
#12496=CARTESIAN_POINT('Ctrl Pts',(6.18974188939196,218.009398692253,4.23955521930249));
#12497=CARTESIAN_POINT('Ctrl Pts',(6.17981026821525,218.002028447915,4.25398300016701));
#12498=CARTESIAN_POINT('Ctrl Pts',(6.09371831161196,217.938139708658,4.37904978050132));
#12499=CARTESIAN_POINT('Ctrl Pts',(6.00362010807817,217.87379055128,4.50180008775267));
#12500=CARTESIAN_POINT('Ctrl Pts',(5.9097213981558,217.809155844927,4.62186318631654));
#12501=CARTESIAN_POINT('Ctrl Pts',(5.81222710407562,217.742046136239,4.74652375992017));
#12502=CARTESIAN_POINT('Ctrl Pts',(5.71063563105773,217.674628800622,4.8682866700552));
#12503=CARTESIAN_POINT('Ctrl Pts',(5.605228561759,217.60710553156,4.98676639590123));
#12504=CARTESIAN_POINT('Ctrl Pts',(5.50372258918827,217.542081286575,5.10086120834527));
#12505=CARTESIAN_POINT('Ctrl Pts',(5.3986788319857,217.476959054234,5.21191112857863));
#12506=CARTESIAN_POINT('Ctrl Pts',(5.29039015693262,217.411920847682,5.31960508912823));
#12507=CARTESIAN_POINT('Ctrl Pts',(5.18212031897114,217.346893954693,5.42728031603836));
#12508=CARTESIAN_POINT('Ctrl Pts',(5.07060708921561,217.281951283188,5.53160039987501));
#12509=CARTESIAN_POINT('Ctrl Pts',(4.95617830276981,217.217273190525,5.63229286774066));
#12510=CARTESIAN_POINT('Ctrl Pts',(4.84171881002289,217.152577741871,5.73301235584603));
#12511=CARTESIAN_POINT('Ctrl Pts',(4.72434264585635,217.088147231022,5.83010200617252));
#12512=CARTESIAN_POINT('Ctrl Pts',(4.60440668292385,217.02415727582,5.92333228977531));
#12513=CARTESIAN_POINT('Ctrl Pts',(4.59057023570477,217.016775056041,5.9340878285374));
#12514=CARTESIAN_POINT('Ctrl Pts',(4.57669974673563,217.009398692253,5.94479205212752));
#12515=CARTESIAN_POINT('Ctrl Pts',(4.56279578422008,217.002028447915,5.95544464740896));
#12516=CARTESIAN_POINT('Ctrl Pts',(4.44226970733684,216.938139708657,6.04778634614857));
#12517=CARTESIAN_POINT('Ctrl Pts',(4.31864929275411,216.87379055128,6.13668694968261));
#12518=CARTESIAN_POINT('Ctrl Pts',(4.19224477495716,216.809155844927,6.22185744482248));
#12519=CARTESIAN_POINT('Ctrl Pts',(4.06099995549857,216.742046136239,6.31028930194794));
#12520=CARTESIAN_POINT('Ctrl Pts',(3.92675391456862,216.674628800622,6.3946992194288));
#12521=CARTESIAN_POINT('Ctrl Pts',(3.78989358567318,216.60710553156,6.47480755900296));
#12522=CARTESIAN_POINT('Ctrl Pts',(3.65809843300166,216.542081286575,6.55195110329844));
#12523=CARTESIAN_POINT('Ctrl Pts',(3.5238795706419,216.476959054234,6.62510554744185));
#12524=CARTESIAN_POINT('Ctrl Pts',(3.38761165659031,216.411920847682,6.69406554949845));
#12525=CARTESIAN_POINT('Ctrl Pts',(3.25136744669046,216.346893954693,6.76301355578654));
#12526=CARTESIAN_POINT('Ctrl Pts',(3.11307538411824,216.281951283188,6.82776836820773));
#12527=CARTESIAN_POINT('Ctrl Pts',(2.97313145734122,216.217273190525,6.88817215625573));
#12528=CARTESIAN_POINT('Ctrl Pts',(2.83314997742261,216.152577741871,6.94859215331013));
#12529=CARTESIAN_POINT('Ctrl Pts',(2.69151625970498,216.088147231022,7.00465866845613));
#12530=CARTESIAN_POINT('Ctrl Pts',(2.54864063859571,216.024157275819,7.0562636864099));
#12531=CARTESIAN_POINT('Ctrl Pts',(2.532157751045,216.016775056041,7.0622171143032));
#12532=CARTESIAN_POINT('Ctrl Pts',(2.51565834512628,216.009398692253,7.06811121908852));
#12533=CARTESIAN_POINT('Ctrl Pts',(2.49914305799789,216.002028447915,7.07394587853975));
#12534=CARTESIAN_POINT('Ctrl Pts',(2.35598079299496,215.938139708658,7.12452344682943));
#12535=CARTESIAN_POINT('Ctrl Pts',(2.2109389948571,215.87379055128,7.17087213616521));
#12536=CARTESIAN_POINT('Ctrl Pts',(2.0644020241,215.809155844927,7.21281294639896));
#12537=CARTESIAN_POINT('Ctrl Pts',(1.91225383662793,215.74204613624,7.25635976072988));
#12538=CARTESIAN_POINT('Ctrl Pts',(1.75849416561922,215.674628800623,7.29515405471512));
#12539=CARTESIAN_POINT('Ctrl Pts',(1.60357741968125,215.607105531561,7.32904944559231));
#12540=CARTESIAN_POINT('Ctrl Pts',(1.4543941147233,215.542081286575,7.3616903741329));
#12541=CARTESIAN_POINT('Ctrl Pts',(1.30413842461201,215.476959054234,7.38978847549662));
#12542=CARTESIAN_POINT('Ctrl Pts',(1.15323012442371,215.411920847683,7.41326423358633));
#12543=CARTESIAN_POINT('Ctrl Pts',(1.00234807511962,215.346893954693,7.43673590800796));
#12544=CARTESIAN_POINT('Ctrl Pts',(0.85081417035265,215.281951283189,7.45558679680064));
#12545=CARTESIAN_POINT('Ctrl Pts',(0.699053789843915,215.217273190525,7.46978916139897));
#12546=CARTESIAN_POINT('Ctrl Pts',(0.547252685316762,215.152577741871,7.4839953371195));
#12547=CARTESIAN_POINT('Ctrl Pts',(0.395225509158773,215.088147231022,7.49355053594384));
#12548=CARTESIAN_POINT('Ctrl Pts',(0.243395891140316,215.02415727582,7.49847882953767));
#12549=CARTESIAN_POINT('Ctrl Pts',(0.225880023133805,215.016775056041,7.49904738356035));
#12550=CARTESIAN_POINT('Ctrl Pts',(0.208366777074288,215.009398692253,7.49955441349819));
#12551=CARTESIAN_POINT('Ctrl Pts',(0.190856796705293,215.002028447915,7.5));
#12552=CARTESIAN_POINT('Ctrl Pts',(0.127311648028422,214.975281229334,7.50161706980302));
#12553=CARTESIAN_POINT('Ctrl Pts',(0.0636823578853861,214.948453397593,
7.50242803155527));
#12554=CARTESIAN_POINT('Ctrl Pts',(-4.068439266928E-7,214.921557632927,
7.50242802810187));
#12555=CARTESIAN_POINT('Origin',(0.,240.,0.));
#12556=CARTESIAN_POINT('Origin',(0.190856796705285,235.002028447915,28.7581985010212));
#12557=CARTESIAN_POINT('',(0.190856796705285,235.002028447915,50.0163970020424));
#12558=CARTESIAN_POINT('Ctrl Pts',(0.190856796705285,235.002028447915,7.5));
#12559=CARTESIAN_POINT('Ctrl Pts',(0.190856796705285,235.002028447915,14.5858638315753));
#12560=CARTESIAN_POINT('Ctrl Pts',(0.190856796705285,235.002028447915,21.6717276631507));
#12561=CARTESIAN_POINT('Ctrl Pts',(0.190856796705285,235.002028447915,35.8438599971648));
#12562=CARTESIAN_POINT('Ctrl Pts',(0.190856796705285,235.002028447915,42.9301284996036));
#12563=CARTESIAN_POINT('Ctrl Pts',(0.190856796705285,235.002028447915,50.0163970020424));
#12564=CARTESIAN_POINT('',(0.000256710972400845,237.995967593475,50.0163970020424));
#12565=CARTESIAN_POINT('',(0.000256710972400879,237.995967593475,50.0163970020424));
#12566=CARTESIAN_POINT('',(0.190856796705286,235.002028447915,50.0163970020424));
#12567=CARTESIAN_POINT('Origin',(0.190856796705285,175.002028447915,28.7581985010212));
#12568=CARTESIAN_POINT('',(0.190856796705285,175.002028447915,50.0163970020424));
#12569=CARTESIAN_POINT('Ctrl Pts',(0.190856796705285,175.002028447915,50.0163970020424));
#12570=CARTESIAN_POINT('Ctrl Pts',(0.190856796705285,175.002028447915,42.9301284996036));
#12571=CARTESIAN_POINT('Ctrl Pts',(0.190856796705285,175.002028447915,35.8438599971648));
#12572=CARTESIAN_POINT('Ctrl Pts',(0.190856796705285,175.002028447915,21.6717276631507));
#12573=CARTESIAN_POINT('Ctrl Pts',(0.190856796705285,175.002028447915,14.5858638315753));
#12574=CARTESIAN_POINT('Ctrl Pts',(0.190856796705285,175.002028447915,7.5));
#12575=CARTESIAN_POINT('',(0.000256710972400845,177.995967593475,50.0163970020424));
#12576=CARTESIAN_POINT('',(0.000256710972401712,177.995967593475,50.0163970020424));
#12577=CARTESIAN_POINT('',(0.00025671097240121,177.995967593475,7.5));
#12578=CARTESIAN_POINT('Ctrl Pts',(0.190856796705285,235.002028447915,7.5));
#12579=CARTESIAN_POINT('Ctrl Pts',(-0.997026505728737,234.502028447915,
7.5302287469283));
#12580=CARTESIAN_POINT('Ctrl Pts',(-2.13611185762632,234.002028447915,7.19190186588755));
#12581=CARTESIAN_POINT('Ctrl Pts',(-3.27519720952391,233.502028447915,6.8535749848468));
#12582=CARTESIAN_POINT('Ctrl Pts',(-4.25398300016701,233.002028447915,6.17981026821526));
#12583=CARTESIAN_POINT('Ctrl Pts',(-5.2327687908101,232.502028447915,5.50604555158371));
#12584=CARTESIAN_POINT('Ctrl Pts',(-5.95544464740896,232.002028447915,4.56279578422009));
#12585=CARTESIAN_POINT('Ctrl Pts',(-6.67812050400781,231.502028447915,3.61954601685647));
#12586=CARTESIAN_POINT('Ctrl Pts',(-7.07394587853975,231.002028447915,2.49914305799789));
#12587=CARTESIAN_POINT('Ctrl Pts',(-7.4697712530717,230.502028447915,1.37874009913931));
#12588=CARTESIAN_POINT('Ctrl Pts',(-7.5,230.002028447915,0.190856796705286));
#12589=CARTESIAN_POINT('Ctrl Pts',(-7.5302287469283,229.502028447915,-0.997026505728736));
#12590=CARTESIAN_POINT('Ctrl Pts',(-7.19190186588755,229.002028447915,-2.13611185762632));
#12591=CARTESIAN_POINT('Ctrl Pts',(-6.8535749848468,228.502028447915,-3.27519720952391));
#12592=CARTESIAN_POINT('Ctrl Pts',(-6.17981026821526,228.002028447915,-4.25398300016701));
#12593=CARTESIAN_POINT('Ctrl Pts',(-5.50604555158371,227.502028447915,-5.2327687908101));
#12594=CARTESIAN_POINT('Ctrl Pts',(-4.56279578422009,227.002028447915,-5.95544464740895));
#12595=CARTESIAN_POINT('Ctrl Pts',(-3.61954601685647,226.502028447915,-6.67812050400781));
#12596=CARTESIAN_POINT('Ctrl Pts',(-2.49914305799789,226.002028447915,-7.07394587853975));
#12597=CARTESIAN_POINT('Ctrl Pts',(-1.37874009913931,225.502028447915,-7.4697712530717));
#12598=CARTESIAN_POINT('Ctrl Pts',(-0.190856796705286,225.002028447915,
-7.5));
#12599=CARTESIAN_POINT('Ctrl Pts',(0.997026505728736,224.502028447915,-7.5302287469283));
#12600=CARTESIAN_POINT('Ctrl Pts',(2.13611185762632,224.002028447915,-7.19190186588755));
#12601=CARTESIAN_POINT('Ctrl Pts',(3.27519720952391,223.502028447915,-6.8535749848468));
#12602=CARTESIAN_POINT('Ctrl Pts',(4.25398300016701,223.002028447915,-6.17981026821526));
#12603=CARTESIAN_POINT('Ctrl Pts',(5.2327687908101,222.502028447915,-5.50604555158371));
#12604=CARTESIAN_POINT('Ctrl Pts',(5.95544464740895,222.002028447915,-4.56279578422009));
#12605=CARTESIAN_POINT('Ctrl Pts',(6.67812050400781,221.502028447915,-3.61954601685647));
#12606=CARTESIAN_POINT('Ctrl Pts',(7.07394587853975,221.002028447915,-2.49914305799789));
#12607=CARTESIAN_POINT('Ctrl Pts',(7.4697712530717,220.502028447915,-1.37874009913931));
#12608=CARTESIAN_POINT('Ctrl Pts',(7.5,220.002028447915,-0.190856796705287));
#12609=CARTESIAN_POINT('Ctrl Pts',(7.5302287469283,219.502028447915,0.997026505728735));
#12610=CARTESIAN_POINT('Ctrl Pts',(7.19190186588755,219.002028447915,2.13611185762632));
#12611=CARTESIAN_POINT('Ctrl Pts',(6.8535749848468,218.502028447915,3.27519720952391));
#12612=CARTESIAN_POINT('Ctrl Pts',(6.17981026821526,218.002028447915,4.25398300016701));
#12613=CARTESIAN_POINT('Ctrl Pts',(5.50604555158371,217.502028447915,5.2327687908101));
#12614=CARTESIAN_POINT('Ctrl Pts',(4.56279578422009,217.002028447915,5.95544464740895));
#12615=CARTESIAN_POINT('Ctrl Pts',(3.61954601685647,216.502028447915,6.67812050400781));
#12616=CARTESIAN_POINT('Ctrl Pts',(2.49914305799789,216.002028447915,7.07394587853975));
#12617=CARTESIAN_POINT('Ctrl Pts',(1.37874009913931,215.502028447915,7.4697712530717));
#12618=CARTESIAN_POINT('Ctrl Pts',(0.190856796705285,215.002028447915,7.5));
#12619=CARTESIAN_POINT('Ctrl Pts',(-0.997026505728737,214.502028447915,
7.5302287469283));
#12620=CARTESIAN_POINT('Ctrl Pts',(-2.13611185762632,214.002028447915,7.19190186588755));
#12621=CARTESIAN_POINT('Ctrl Pts',(-3.27519720952391,213.502028447915,6.8535749848468));
#12622=CARTESIAN_POINT('Ctrl Pts',(-4.25398300016701,213.002028447915,6.17981026821526));
#12623=CARTESIAN_POINT('Ctrl Pts',(-5.2327687908101,212.502028447915,5.50604555158371));
#12624=CARTESIAN_POINT('Ctrl Pts',(-5.95544464740896,212.002028447915,4.56279578422009));
#12625=CARTESIAN_POINT('Ctrl Pts',(-6.67812050400781,211.502028447915,3.61954601685647));
#12626=CARTESIAN_POINT('Ctrl Pts',(-7.07394587853975,211.002028447915,2.49914305799789));
#12627=CARTESIAN_POINT('Ctrl Pts',(-7.4697712530717,210.502028447915,1.37874009913931));
#12628=CARTESIAN_POINT('Ctrl Pts',(-7.5,210.002028447915,0.190856796705286));
#12629=CARTESIAN_POINT('Ctrl Pts',(-7.5302287469283,209.502028447915,-0.997026505728736));
#12630=CARTESIAN_POINT('Ctrl Pts',(-7.19190186588755,209.002028447915,-2.13611185762632));
#12631=CARTESIAN_POINT('Ctrl Pts',(-6.8535749848468,208.502028447915,-3.27519720952391));
#12632=CARTESIAN_POINT('Ctrl Pts',(-6.17981026821526,208.002028447915,-4.25398300016701));
#12633=CARTESIAN_POINT('Ctrl Pts',(-5.50604555158371,207.502028447915,-5.2327687908101));
#12634=CARTESIAN_POINT('Ctrl Pts',(-4.56279578422009,207.002028447915,-5.95544464740895));
#12635=CARTESIAN_POINT('Ctrl Pts',(-3.61954601685647,206.502028447915,-6.67812050400781));
#12636=CARTESIAN_POINT('Ctrl Pts',(-2.49914305799789,206.002028447915,-7.07394587853975));
#12637=CARTESIAN_POINT('Ctrl Pts',(-1.37874009913931,205.502028447915,-7.4697712530717));
#12638=CARTESIAN_POINT('Ctrl Pts',(-0.190856796705286,205.002028447915,
-7.5));
#12639=CARTESIAN_POINT('Ctrl Pts',(0.997026505728736,204.502028447915,-7.5302287469283));
#12640=CARTESIAN_POINT('Ctrl Pts',(2.13611185762632,204.002028447915,-7.19190186588755));
#12641=CARTESIAN_POINT('Ctrl Pts',(3.27519720952391,203.502028447915,-6.8535749848468));
#12642=CARTESIAN_POINT('Ctrl Pts',(4.25398300016701,203.002028447915,-6.17981026821526));
#12643=CARTESIAN_POINT('Ctrl Pts',(5.2327687908101,202.502028447915,-5.50604555158371));
#12644=CARTESIAN_POINT('Ctrl Pts',(5.95544464740895,202.002028447915,-4.56279578422009));
#12645=CARTESIAN_POINT('Ctrl Pts',(6.67812050400781,201.502028447915,-3.61954601685647));
#12646=CARTESIAN_POINT('Ctrl Pts',(7.07394587853975,201.002028447915,-2.49914305799789));
#12647=CARTESIAN_POINT('Ctrl Pts',(7.4697712530717,200.502028447915,-1.37874009913931));
#12648=CARTESIAN_POINT('Ctrl Pts',(7.5,200.002028447915,-0.190856796705287));
#12649=CARTESIAN_POINT('Ctrl Pts',(7.5302287469283,199.502028447915,0.997026505728735));
#12650=CARTESIAN_POINT('Ctrl Pts',(7.19190186588755,199.002028447915,2.13611185762632));
#12651=CARTESIAN_POINT('Ctrl Pts',(6.8535749848468,198.502028447915,3.27519720952391));
#12652=CARTESIAN_POINT('Ctrl Pts',(6.17981026821526,198.002028447915,4.25398300016701));
#12653=CARTESIAN_POINT('Ctrl Pts',(5.50604555158371,197.502028447915,5.2327687908101));
#12654=CARTESIAN_POINT('Ctrl Pts',(4.56279578422009,197.002028447915,5.95544464740895));
#12655=CARTESIAN_POINT('Ctrl Pts',(3.61954601685647,196.502028447915,6.67812050400781));
#12656=CARTESIAN_POINT('Ctrl Pts',(2.49914305799789,196.002028447915,7.07394587853975));
#12657=CARTESIAN_POINT('Ctrl Pts',(1.37874009913931,195.502028447915,7.4697712530717));
#12658=CARTESIAN_POINT('Ctrl Pts',(0.190856796705285,195.002028447915,7.5));
#12659=CARTESIAN_POINT('Ctrl Pts',(-0.997026505728737,194.502028447915,
7.5302287469283));
#12660=CARTESIAN_POINT('Ctrl Pts',(-2.13611185762632,194.002028447915,7.19190186588755));
#12661=CARTESIAN_POINT('Ctrl Pts',(-3.27519720952391,193.502028447915,6.8535749848468));
#12662=CARTESIAN_POINT('Ctrl Pts',(-4.25398300016701,193.002028447915,6.17981026821526));
#12663=CARTESIAN_POINT('Ctrl Pts',(-5.2327687908101,192.502028447915,5.50604555158371));
#12664=CARTESIAN_POINT('Ctrl Pts',(-5.95544464740896,192.002028447915,4.56279578422009));
#12665=CARTESIAN_POINT('Ctrl Pts',(-6.67812050400781,191.502028447915,3.61954601685647));
#12666=CARTESIAN_POINT('Ctrl Pts',(-7.07394587853975,191.002028447915,2.49914305799789));
#12667=CARTESIAN_POINT('Ctrl Pts',(-7.4697712530717,190.502028447915,1.37874009913931));
#12668=CARTESIAN_POINT('Ctrl Pts',(-7.5,190.002028447915,0.190856796705286));
#12669=CARTESIAN_POINT('Ctrl Pts',(-7.5302287469283,189.502028447915,-0.997026505728736));
#12670=CARTESIAN_POINT('Ctrl Pts',(-7.19190186588755,189.002028447915,-2.13611185762632));
#12671=CARTESIAN_POINT('Ctrl Pts',(-6.8535749848468,188.502028447915,-3.27519720952391));
#12672=CARTESIAN_POINT('Ctrl Pts',(-6.17981026821526,188.002028447915,-4.25398300016701));
#12673=CARTESIAN_POINT('Ctrl Pts',(-5.50604555158371,187.502028447915,-5.2327687908101));
#12674=CARTESIAN_POINT('Ctrl Pts',(-4.56279578422009,187.002028447915,-5.95544464740895));
#12675=CARTESIAN_POINT('Ctrl Pts',(-3.61954601685647,186.502028447915,-6.67812050400781));
#12676=CARTESIAN_POINT('Ctrl Pts',(-2.49914305799789,186.002028447915,-7.07394587853975));
#12677=CARTESIAN_POINT('Ctrl Pts',(-1.37874009913931,185.502028447915,-7.4697712530717));
#12678=CARTESIAN_POINT('Ctrl Pts',(-0.190856796705286,185.002028447915,
-7.5));
#12679=CARTESIAN_POINT('Ctrl Pts',(0.997026505728736,184.502028447915,-7.5302287469283));
#12680=CARTESIAN_POINT('Ctrl Pts',(2.13611185762632,184.002028447915,-7.19190186588755));
#12681=CARTESIAN_POINT('Ctrl Pts',(3.27519720952391,183.502028447915,-6.8535749848468));
#12682=CARTESIAN_POINT('Ctrl Pts',(4.25398300016701,183.002028447915,-6.17981026821526));
#12683=CARTESIAN_POINT('Ctrl Pts',(5.2327687908101,182.502028447915,-5.50604555158371));
#12684=CARTESIAN_POINT('Ctrl Pts',(5.95544464740895,182.002028447915,-4.56279578422009));
#12685=CARTESIAN_POINT('Ctrl Pts',(6.67812050400781,181.502028447915,-3.61954601685647));
#12686=CARTESIAN_POINT('Ctrl Pts',(7.07394587853975,181.002028447915,-2.49914305799789));
#12687=CARTESIAN_POINT('Ctrl Pts',(7.4697712530717,180.502028447915,-1.37874009913931));
#12688=CARTESIAN_POINT('Ctrl Pts',(7.5,180.002028447915,-0.190856796705287));
#12689=CARTESIAN_POINT('Ctrl Pts',(7.5302287469283,179.502028447915,0.997026505728735));
#12690=CARTESIAN_POINT('Ctrl Pts',(7.19190186588755,179.002028447915,2.13611185762632));
#12691=CARTESIAN_POINT('Ctrl Pts',(6.8535749848468,178.502028447915,3.27519720952391));
#12692=CARTESIAN_POINT('Ctrl Pts',(6.17981026821526,178.002028447915,4.25398300016701));
#12693=CARTESIAN_POINT('Ctrl Pts',(5.50604555158371,177.502028447915,5.2327687908101));
#12694=CARTESIAN_POINT('Ctrl Pts',(4.56279578422009,177.002028447915,5.95544464740895));
#12695=CARTESIAN_POINT('Ctrl Pts',(3.61954601685647,176.502028447915,6.67812050400781));
#12696=CARTESIAN_POINT('Ctrl Pts',(2.49914305799789,176.002028447915,7.07394587853975));
#12697=CARTESIAN_POINT('Ctrl Pts',(1.37874009913931,175.502028447915,7.4697712530717));
#12698=CARTESIAN_POINT('Ctrl Pts',(0.190856796705285,175.002028447915,7.5));
#12699=CARTESIAN_POINT('Ctrl Pts',(0.190856796705285,235.002028447915,50.0163970020424));
#12700=CARTESIAN_POINT('Ctrl Pts',(-7.73096224951301,234.502028447915,50.0466257489707));
#12701=CARTESIAN_POINT('Ctrl Pts',(-15.2744010708495,234.002028447915,47.6273982840717));
#12702=CARTESIAN_POINT('Ctrl Pts',(-22.817839892186,233.502028447915,45.2081708191727));
#12703=CARTESIAN_POINT('Ctrl Pts',(-29.2444941385794,233.002028447915,40.5762979824596));
#12704=CARTESIAN_POINT('Ctrl Pts',(-35.6711483849729,232.502028447915,35.9444251457465));
#12705=CARTESIAN_POINT('Ctrl Pts',(-40.3519323616533,232.002028447915,29.5533069226325));
#12706=CARTESIAN_POINT('Ctrl Pts',(-45.0327163383337,231.502028447915,23.1621886995185));
#12707=CARTESIAN_POINT('Ctrl Pts',(-47.5094422967239,231.002028447915,15.6374322712211));
#12708=CARTESIAN_POINT('Ctrl Pts',(-49.9861682551141,230.502028447915,8.11267584292358));
#12709=CARTESIAN_POINT('Ctrl Pts',(-50.0163970020424,230.002028447915,0.190856796705288));
#12710=CARTESIAN_POINT('Ctrl Pts',(-50.0466257489707,229.502028447915,-7.73096224951301));
#12711=CARTESIAN_POINT('Ctrl Pts',(-47.6273982840717,229.002028447915,-15.2744010708495));
#12712=CARTESIAN_POINT('Ctrl Pts',(-45.2081708191727,228.502028447915,-22.817839892186));
#12713=CARTESIAN_POINT('Ctrl Pts',(-40.5762979824596,228.002028447915,-29.2444941385794));
#12714=CARTESIAN_POINT('Ctrl Pts',(-35.9444251457465,227.502028447915,-35.6711483849729));
#12715=CARTESIAN_POINT('Ctrl Pts',(-29.5533069226325,227.002028447915,-40.3519323616533));
#12716=CARTESIAN_POINT('Ctrl Pts',(-23.1621886995185,226.502028447915,-45.0327163383337));
#12717=CARTESIAN_POINT('Ctrl Pts',(-15.6374322712211,226.002028447915,-47.5094422967239));
#12718=CARTESIAN_POINT('Ctrl Pts',(-8.11267584292359,225.502028447915,-49.9861682551141));
#12719=CARTESIAN_POINT('Ctrl Pts',(-0.190856796705292,225.002028447915,
-50.0163970020424));
#12720=CARTESIAN_POINT('Ctrl Pts',(7.730962249513,224.502028447915,-50.0466257489707));
#12721=CARTESIAN_POINT('Ctrl Pts',(15.2744010708495,224.002028447915,-47.6273982840717));
#12722=CARTESIAN_POINT('Ctrl Pts',(22.817839892186,223.502028447915,-45.2081708191727));
#12723=CARTESIAN_POINT('Ctrl Pts',(29.2444941385794,223.002028447915,-40.5762979824596));
#12724=CARTESIAN_POINT('Ctrl Pts',(35.6711483849729,222.502028447915,-35.9444251457465));
#12725=CARTESIAN_POINT('Ctrl Pts',(40.3519323616533,222.002028447915,-29.5533069226325));
#12726=CARTESIAN_POINT('Ctrl Pts',(45.0327163383337,221.502028447915,-23.1621886995185));
#12727=CARTESIAN_POINT('Ctrl Pts',(47.5094422967239,221.002028447915,-15.6374322712211));
#12728=CARTESIAN_POINT('Ctrl Pts',(49.9861682551141,220.502028447915,-8.11267584292359));
#12729=CARTESIAN_POINT('Ctrl Pts',(50.0163970020424,220.002028447915,-0.190856796705295));
#12730=CARTESIAN_POINT('Ctrl Pts',(50.0466257489707,219.502028447915,7.730962249513));
#12731=CARTESIAN_POINT('Ctrl Pts',(47.6273982840717,219.002028447915,15.2744010708495));
#12732=CARTESIAN_POINT('Ctrl Pts',(45.2081708191727,218.502028447915,22.817839892186));
#12733=CARTESIAN_POINT('Ctrl Pts',(40.5762979824596,218.002028447915,29.2444941385794));
#12734=CARTESIAN_POINT('Ctrl Pts',(35.9444251457465,217.502028447915,35.6711483849729));
#12735=CARTESIAN_POINT('Ctrl Pts',(29.5533069226325,217.002028447915,40.3519323616533));
#12736=CARTESIAN_POINT('Ctrl Pts',(23.1621886995185,216.502028447915,45.0327163383337));
#12737=CARTESIAN_POINT('Ctrl Pts',(15.6374322712211,216.002028447915,47.5094422967239));
#12738=CARTESIAN_POINT('Ctrl Pts',(8.11267584292359,215.502028447915,49.9861682551141));
#12739=CARTESIAN_POINT('Ctrl Pts',(0.190856796705285,215.002028447915,50.0163970020424));
#12740=CARTESIAN_POINT('Ctrl Pts',(-7.73096224951301,214.502028447915,50.0466257489707));
#12741=CARTESIAN_POINT('Ctrl Pts',(-15.2744010708495,214.002028447915,47.6273982840717));
#12742=CARTESIAN_POINT('Ctrl Pts',(-22.817839892186,213.502028447915,45.2081708191727));
#12743=CARTESIAN_POINT('Ctrl Pts',(-29.2444941385794,213.002028447915,40.5762979824596));
#12744=CARTESIAN_POINT('Ctrl Pts',(-35.6711483849729,212.502028447915,35.9444251457465));
#12745=CARTESIAN_POINT('Ctrl Pts',(-40.3519323616533,212.002028447915,29.5533069226325));
#12746=CARTESIAN_POINT('Ctrl Pts',(-45.0327163383337,211.502028447915,23.1621886995185));
#12747=CARTESIAN_POINT('Ctrl Pts',(-47.5094422967239,211.002028447915,15.6374322712211));
#12748=CARTESIAN_POINT('Ctrl Pts',(-49.9861682551141,210.502028447915,8.11267584292358));
#12749=CARTESIAN_POINT('Ctrl Pts',(-50.0163970020424,210.002028447915,0.190856796705288));
#12750=CARTESIAN_POINT('Ctrl Pts',(-50.0466257489707,209.502028447915,-7.73096224951301));
#12751=CARTESIAN_POINT('Ctrl Pts',(-47.6273982840717,209.002028447915,-15.2744010708495));
#12752=CARTESIAN_POINT('Ctrl Pts',(-45.2081708191727,208.502028447915,-22.817839892186));
#12753=CARTESIAN_POINT('Ctrl Pts',(-40.5762979824596,208.002028447915,-29.2444941385794));
#12754=CARTESIAN_POINT('Ctrl Pts',(-35.9444251457465,207.502028447915,-35.6711483849729));
#12755=CARTESIAN_POINT('Ctrl Pts',(-29.5533069226325,207.002028447915,-40.3519323616533));
#12756=CARTESIAN_POINT('Ctrl Pts',(-23.1621886995185,206.502028447915,-45.0327163383337));
#12757=CARTESIAN_POINT('Ctrl Pts',(-15.6374322712211,206.002028447915,-47.5094422967239));
#12758=CARTESIAN_POINT('Ctrl Pts',(-8.11267584292359,205.502028447915,-49.9861682551141));
#12759=CARTESIAN_POINT('Ctrl Pts',(-0.190856796705292,205.002028447915,
-50.0163970020424));
#12760=CARTESIAN_POINT('Ctrl Pts',(7.730962249513,204.502028447915,-50.0466257489707));
#12761=CARTESIAN_POINT('Ctrl Pts',(15.2744010708495,204.002028447915,-47.6273982840717));
#12762=CARTESIAN_POINT('Ctrl Pts',(22.817839892186,203.502028447915,-45.2081708191727));
#12763=CARTESIAN_POINT('Ctrl Pts',(29.2444941385794,203.002028447915,-40.5762979824596));
#12764=CARTESIAN_POINT('Ctrl Pts',(35.6711483849729,202.502028447915,-35.9444251457465));
#12765=CARTESIAN_POINT('Ctrl Pts',(40.3519323616533,202.002028447915,-29.5533069226325));
#12766=CARTESIAN_POINT('Ctrl Pts',(45.0327163383337,201.502028447915,-23.1621886995185));
#12767=CARTESIAN_POINT('Ctrl Pts',(47.5094422967239,201.002028447915,-15.6374322712211));
#12768=CARTESIAN_POINT('Ctrl Pts',(49.9861682551141,200.502028447915,-8.11267584292359));
#12769=CARTESIAN_POINT('Ctrl Pts',(50.0163970020424,200.002028447915,-0.190856796705295));
#12770=CARTESIAN_POINT('Ctrl Pts',(50.0466257489707,199.502028447915,7.730962249513));
#12771=CARTESIAN_POINT('Ctrl Pts',(47.6273982840717,199.002028447915,15.2744010708495));
#12772=CARTESIAN_POINT('Ctrl Pts',(45.2081708191727,198.502028447915,22.817839892186));
#12773=CARTESIAN_POINT('Ctrl Pts',(40.5762979824596,198.002028447915,29.2444941385794));
#12774=CARTESIAN_POINT('Ctrl Pts',(35.9444251457465,197.502028447915,35.6711483849729));
#12775=CARTESIAN_POINT('Ctrl Pts',(29.5533069226325,197.002028447915,40.3519323616533));
#12776=CARTESIAN_POINT('Ctrl Pts',(23.1621886995185,196.502028447915,45.0327163383337));
#12777=CARTESIAN_POINT('Ctrl Pts',(15.6374322712211,196.002028447915,47.5094422967239));
#12778=CARTESIAN_POINT('Ctrl Pts',(8.11267584292359,195.502028447915,49.9861682551141));
#12779=CARTESIAN_POINT('Ctrl Pts',(0.190856796705285,195.002028447915,50.0163970020424));
#12780=CARTESIAN_POINT('Ctrl Pts',(-7.73096224951301,194.502028447915,50.0466257489707));
#12781=CARTESIAN_POINT('Ctrl Pts',(-15.2744010708495,194.002028447915,47.6273982840717));
#12782=CARTESIAN_POINT('Ctrl Pts',(-22.817839892186,193.502028447915,45.2081708191727));
#12783=CARTESIAN_POINT('Ctrl Pts',(-29.2444941385794,193.002028447915,40.5762979824596));
#12784=CARTESIAN_POINT('Ctrl Pts',(-35.6711483849729,192.502028447915,35.9444251457465));
#12785=CARTESIAN_POINT('Ctrl Pts',(-40.3519323616533,192.002028447915,29.5533069226325));
#12786=CARTESIAN_POINT('Ctrl Pts',(-45.0327163383337,191.502028447915,23.1621886995185));
#12787=CARTESIAN_POINT('Ctrl Pts',(-47.5094422967239,191.002028447915,15.6374322712211));
#12788=CARTESIAN_POINT('Ctrl Pts',(-49.9861682551141,190.502028447915,8.11267584292358));
#12789=CARTESIAN_POINT('Ctrl Pts',(-50.0163970020424,190.002028447915,0.190856796705288));
#12790=CARTESIAN_POINT('Ctrl Pts',(-50.0466257489707,189.502028447915,-7.73096224951301));
#12791=CARTESIAN_POINT('Ctrl Pts',(-47.6273982840717,189.002028447915,-15.2744010708495));
#12792=CARTESIAN_POINT('Ctrl Pts',(-45.2081708191727,188.502028447915,-22.817839892186));
#12793=CARTESIAN_POINT('Ctrl Pts',(-40.5762979824596,188.002028447915,-29.2444941385794));
#12794=CARTESIAN_POINT('Ctrl Pts',(-35.9444251457465,187.502028447915,-35.6711483849729));
#12795=CARTESIAN_POINT('Ctrl Pts',(-29.5533069226325,187.002028447915,-40.3519323616533));
#12796=CARTESIAN_POINT('Ctrl Pts',(-23.1621886995185,186.502028447915,-45.0327163383337));
#12797=CARTESIAN_POINT('Ctrl Pts',(-15.6374322712211,186.002028447915,-47.5094422967239));
#12798=CARTESIAN_POINT('Ctrl Pts',(-8.11267584292359,185.502028447915,-49.9861682551141));
#12799=CARTESIAN_POINT('Ctrl Pts',(-0.190856796705292,185.002028447915,
-50.0163970020424));
#12800=CARTESIAN_POINT('Ctrl Pts',(7.730962249513,184.502028447915,-50.0466257489707));
#12801=CARTESIAN_POINT('Ctrl Pts',(15.2744010708495,184.002028447915,-47.6273982840717));
#12802=CARTESIAN_POINT('Ctrl Pts',(22.817839892186,183.502028447915,-45.2081708191727));
#12803=CARTESIAN_POINT('Ctrl Pts',(29.2444941385794,183.002028447915,-40.5762979824596));
#12804=CARTESIAN_POINT('Ctrl Pts',(35.6711483849729,182.502028447915,-35.9444251457465));
#12805=CARTESIAN_POINT('Ctrl Pts',(40.3519323616533,182.002028447915,-29.5533069226325));
#12806=CARTESIAN_POINT('Ctrl Pts',(45.0327163383337,181.502028447915,-23.1621886995185));
#12807=CARTESIAN_POINT('Ctrl Pts',(47.5094422967239,181.002028447915,-15.6374322712211));
#12808=CARTESIAN_POINT('Ctrl Pts',(49.9861682551141,180.502028447915,-8.11267584292359));
#12809=CARTESIAN_POINT('Ctrl Pts',(50.0163970020424,180.002028447915,-0.190856796705295));
#12810=CARTESIAN_POINT('Ctrl Pts',(50.0466257489707,179.502028447915,7.730962249513));
#12811=CARTESIAN_POINT('Ctrl Pts',(47.6273982840717,179.002028447915,15.2744010708495));
#12812=CARTESIAN_POINT('Ctrl Pts',(45.2081708191727,178.502028447915,22.817839892186));
#12813=CARTESIAN_POINT('Ctrl Pts',(40.5762979824596,178.002028447915,29.2444941385794));
#12814=CARTESIAN_POINT('Ctrl Pts',(35.9444251457465,177.502028447915,35.6711483849729));
#12815=CARTESIAN_POINT('Ctrl Pts',(29.5533069226325,177.002028447915,40.3519323616533));
#12816=CARTESIAN_POINT('Ctrl Pts',(23.1621886995185,176.502028447915,45.0327163383337));
#12817=CARTESIAN_POINT('Ctrl Pts',(15.6374322712211,176.002028447915,47.5094422967239));
#12818=CARTESIAN_POINT('Ctrl Pts',(8.11267584292359,175.502028447915,49.9861682551141));
#12819=CARTESIAN_POINT('Ctrl Pts',(0.190856796705285,175.002028447915,50.0163970020424));
#12820=CARTESIAN_POINT('Ctrl Pts',(0.190856796705285,235.002028447915,50.0163970020424));
#12821=CARTESIAN_POINT('Ctrl Pts',(-7.73096224951301,234.502028447915,50.0466257489707));
#12822=CARTESIAN_POINT('Ctrl Pts',(-15.2744010708495,234.002028447915,47.6273982840717));
#12823=CARTESIAN_POINT('Ctrl Pts',(-22.817839892186,233.502028447915,45.2081708191727));
#12824=CARTESIAN_POINT('Ctrl Pts',(-29.2444941385794,233.002028447915,40.5762979824596));
#12825=CARTESIAN_POINT('Ctrl Pts',(-35.6711483849729,232.502028447915,35.9444251457465));
#12826=CARTESIAN_POINT('Ctrl Pts',(-40.3519323616533,232.002028447915,29.5533069226325));
#12827=CARTESIAN_POINT('Ctrl Pts',(-45.0327163383337,231.502028447915,23.1621886995185));
#12828=CARTESIAN_POINT('Ctrl Pts',(-47.5094422967239,231.002028447915,15.6374322712211));
#12829=CARTESIAN_POINT('Ctrl Pts',(-49.9861682551141,230.502028447915,8.11267584292358));
#12830=CARTESIAN_POINT('Ctrl Pts',(-50.0163970020424,230.002028447915,0.190856796705288));
#12831=CARTESIAN_POINT('Ctrl Pts',(-50.0466257489707,229.502028447915,-7.73096224951301));
#12832=CARTESIAN_POINT('Ctrl Pts',(-47.6273982840717,229.002028447915,-15.2744010708495));
#12833=CARTESIAN_POINT('Ctrl Pts',(-45.2081708191727,228.502028447915,-22.817839892186));
#12834=CARTESIAN_POINT('Ctrl Pts',(-40.5762979824596,228.002028447915,-29.2444941385794));
#12835=CARTESIAN_POINT('Ctrl Pts',(-35.9444251457465,227.502028447915,-35.6711483849729));
#12836=CARTESIAN_POINT('Ctrl Pts',(-29.5533069226325,227.002028447915,-40.3519323616533));
#12837=CARTESIAN_POINT('Ctrl Pts',(-23.1621886995185,226.502028447915,-45.0327163383337));
#12838=CARTESIAN_POINT('Ctrl Pts',(-15.6374322712211,226.002028447915,-47.5094422967239));
#12839=CARTESIAN_POINT('Ctrl Pts',(-8.11267584292359,225.502028447915,-49.9861682551141));
#12840=CARTESIAN_POINT('Ctrl Pts',(-0.190856796705292,225.002028447915,
-50.0163970020424));
#12841=CARTESIAN_POINT('Ctrl Pts',(7.730962249513,224.502028447915,-50.0466257489707));
#12842=CARTESIAN_POINT('Ctrl Pts',(15.2744010708495,224.002028447915,-47.6273982840717));
#12843=CARTESIAN_POINT('Ctrl Pts',(22.817839892186,223.502028447915,-45.2081708191727));
#12844=CARTESIAN_POINT('Ctrl Pts',(29.2444941385794,223.002028447915,-40.5762979824596));
#12845=CARTESIAN_POINT('Ctrl Pts',(35.6711483849729,222.502028447915,-35.9444251457465));
#12846=CARTESIAN_POINT('Ctrl Pts',(40.3519323616533,222.002028447915,-29.5533069226325));
#12847=CARTESIAN_POINT('Ctrl Pts',(45.0327163383337,221.502028447915,-23.1621886995185));
#12848=CARTESIAN_POINT('Ctrl Pts',(47.5094422967239,221.002028447915,-15.6374322712211));
#12849=CARTESIAN_POINT('Ctrl Pts',(49.9861682551141,220.502028447915,-8.11267584292359));
#12850=CARTESIAN_POINT('Ctrl Pts',(50.0163970020424,220.002028447915,-0.190856796705295));
#12851=CARTESIAN_POINT('Ctrl Pts',(50.0466257489707,219.502028447915,7.730962249513));
#12852=CARTESIAN_POINT('Ctrl Pts',(47.6273982840717,219.002028447915,15.2744010708495));
#12853=CARTESIAN_POINT('Ctrl Pts',(45.2081708191727,218.502028447915,22.817839892186));
#12854=CARTESIAN_POINT('Ctrl Pts',(40.5762979824596,218.002028447915,29.2444941385794));
#12855=CARTESIAN_POINT('Ctrl Pts',(35.9444251457465,217.502028447915,35.6711483849729));
#12856=CARTESIAN_POINT('Ctrl Pts',(29.5533069226325,217.002028447915,40.3519323616533));
#12857=CARTESIAN_POINT('Ctrl Pts',(23.1621886995185,216.502028447915,45.0327163383337));
#12858=CARTESIAN_POINT('Ctrl Pts',(15.6374322712211,216.002028447915,47.5094422967239));
#12859=CARTESIAN_POINT('Ctrl Pts',(8.11267584292359,215.502028447915,49.9861682551141));
#12860=CARTESIAN_POINT('Ctrl Pts',(0.190856796705285,215.002028447915,50.0163970020424));
#12861=CARTESIAN_POINT('Ctrl Pts',(-7.73096224951301,214.502028447915,50.0466257489707));
#12862=CARTESIAN_POINT('Ctrl Pts',(-15.2744010708495,214.002028447915,47.6273982840717));
#12863=CARTESIAN_POINT('Ctrl Pts',(-22.817839892186,213.502028447915,45.2081708191727));
#12864=CARTESIAN_POINT('Ctrl Pts',(-29.2444941385794,213.002028447915,40.5762979824596));
#12865=CARTESIAN_POINT('Ctrl Pts',(-35.6711483849729,212.502028447915,35.9444251457465));
#12866=CARTESIAN_POINT('Ctrl Pts',(-40.3519323616533,212.002028447915,29.5533069226325));
#12867=CARTESIAN_POINT('Ctrl Pts',(-45.0327163383337,211.502028447915,23.1621886995185));
#12868=CARTESIAN_POINT('Ctrl Pts',(-47.5094422967239,211.002028447915,15.6374322712211));
#12869=CARTESIAN_POINT('Ctrl Pts',(-49.9861682551141,210.502028447915,8.11267584292358));
#12870=CARTESIAN_POINT('Ctrl Pts',(-50.0163970020424,210.002028447915,0.190856796705288));
#12871=CARTESIAN_POINT('Ctrl Pts',(-50.0466257489707,209.502028447915,-7.73096224951301));
#12872=CARTESIAN_POINT('Ctrl Pts',(-47.6273982840717,209.002028447915,-15.2744010708495));
#12873=CARTESIAN_POINT('Ctrl Pts',(-45.2081708191727,208.502028447915,-22.817839892186));
#12874=CARTESIAN_POINT('Ctrl Pts',(-40.5762979824596,208.002028447915,-29.2444941385794));
#12875=CARTESIAN_POINT('Ctrl Pts',(-35.9444251457465,207.502028447915,-35.6711483849729));
#12876=CARTESIAN_POINT('Ctrl Pts',(-29.5533069226325,207.002028447915,-40.3519323616533));
#12877=CARTESIAN_POINT('Ctrl Pts',(-23.1621886995185,206.502028447915,-45.0327163383337));
#12878=CARTESIAN_POINT('Ctrl Pts',(-15.6374322712211,206.002028447915,-47.5094422967239));
#12879=CARTESIAN_POINT('Ctrl Pts',(-8.11267584292359,205.502028447915,-49.9861682551141));
#12880=CARTESIAN_POINT('Ctrl Pts',(-0.190856796705292,205.002028447915,
-50.0163970020424));
#12881=CARTESIAN_POINT('Ctrl Pts',(7.730962249513,204.502028447915,-50.0466257489707));
#12882=CARTESIAN_POINT('Ctrl Pts',(15.2744010708495,204.002028447915,-47.6273982840717));
#12883=CARTESIAN_POINT('Ctrl Pts',(22.817839892186,203.502028447915,-45.2081708191727));
#12884=CARTESIAN_POINT('Ctrl Pts',(29.2444941385794,203.002028447915,-40.5762979824596));
#12885=CARTESIAN_POINT('Ctrl Pts',(35.6711483849729,202.502028447915,-35.9444251457465));
#12886=CARTESIAN_POINT('Ctrl Pts',(40.3519323616533,202.002028447915,-29.5533069226325));
#12887=CARTESIAN_POINT('Ctrl Pts',(45.0327163383337,201.502028447915,-23.1621886995185));
#12888=CARTESIAN_POINT('Ctrl Pts',(47.5094422967239,201.002028447915,-15.6374322712211));
#12889=CARTESIAN_POINT('Ctrl Pts',(49.9861682551141,200.502028447915,-8.11267584292359));
#12890=CARTESIAN_POINT('Ctrl Pts',(50.0163970020424,200.002028447915,-0.190856796705295));
#12891=CARTESIAN_POINT('Ctrl Pts',(50.0466257489707,199.502028447915,7.730962249513));
#12892=CARTESIAN_POINT('Ctrl Pts',(47.6273982840717,199.002028447915,15.2744010708495));
#12893=CARTESIAN_POINT('Ctrl Pts',(45.2081708191727,198.502028447915,22.817839892186));
#12894=CARTESIAN_POINT('Ctrl Pts',(40.5762979824596,198.002028447915,29.2444941385794));
#12895=CARTESIAN_POINT('Ctrl Pts',(35.9444251457465,197.502028447915,35.6711483849729));
#12896=CARTESIAN_POINT('Ctrl Pts',(29.5533069226325,197.002028447915,40.3519323616533));
#12897=CARTESIAN_POINT('Ctrl Pts',(23.1621886995185,196.502028447915,45.0327163383337));
#12898=CARTESIAN_POINT('Ctrl Pts',(15.6374322712211,196.002028447915,47.5094422967239));
#12899=CARTESIAN_POINT('Ctrl Pts',(8.11267584292359,195.502028447915,49.9861682551141));
#12900=CARTESIAN_POINT('Ctrl Pts',(0.190856796705285,195.002028447915,50.0163970020424));
#12901=CARTESIAN_POINT('Ctrl Pts',(-7.73096224951301,194.502028447915,50.0466257489707));
#12902=CARTESIAN_POINT('Ctrl Pts',(-15.2744010708495,194.002028447915,47.6273982840717));
#12903=CARTESIAN_POINT('Ctrl Pts',(-22.817839892186,193.502028447915,45.2081708191727));
#12904=CARTESIAN_POINT('Ctrl Pts',(-29.2444941385794,193.002028447915,40.5762979824596));
#12905=CARTESIAN_POINT('Ctrl Pts',(-35.6711483849729,192.502028447915,35.9444251457465));
#12906=CARTESIAN_POINT('Ctrl Pts',(-40.3519323616533,192.002028447915,29.5533069226325));
#12907=CARTESIAN_POINT('Ctrl Pts',(-45.0327163383337,191.502028447915,23.1621886995185));
#12908=CARTESIAN_POINT('Ctrl Pts',(-47.5094422967239,191.002028447915,15.6374322712211));
#12909=CARTESIAN_POINT('Ctrl Pts',(-49.9861682551141,190.502028447915,8.11267584292358));
#12910=CARTESIAN_POINT('Ctrl Pts',(-50.0163970020424,190.002028447915,0.190856796705288));
#12911=CARTESIAN_POINT('Ctrl Pts',(-50.0466257489707,189.502028447915,-7.73096224951301));
#12912=CARTESIAN_POINT('Ctrl Pts',(-47.6273982840717,189.002028447915,-15.2744010708495));
#12913=CARTESIAN_POINT('Ctrl Pts',(-45.2081708191727,188.502028447915,-22.817839892186));
#12914=CARTESIAN_POINT('Ctrl Pts',(-40.5762979824596,188.002028447915,-29.2444941385794));
#12915=CARTESIAN_POINT('Ctrl Pts',(-35.9444251457465,187.502028447915,-35.6711483849729));
#12916=CARTESIAN_POINT('Ctrl Pts',(-29.5533069226325,187.002028447915,-40.3519323616533));
#12917=CARTESIAN_POINT('Ctrl Pts',(-23.1621886995185,186.502028447915,-45.0327163383337));
#12918=CARTESIAN_POINT('Ctrl Pts',(-15.6374322712211,186.002028447915,-47.5094422967239));
#12919=CARTESIAN_POINT('Ctrl Pts',(-8.11267584292359,185.502028447915,-49.9861682551141));
#12920=CARTESIAN_POINT('Ctrl Pts',(-0.190856796705292,185.002028447915,
-50.0163970020424));
#12921=CARTESIAN_POINT('Ctrl Pts',(7.730962249513,184.502028447915,-50.0466257489707));
#12922=CARTESIAN_POINT('Ctrl Pts',(15.2744010708495,184.002028447915,-47.6273982840717));
#12923=CARTESIAN_POINT('Ctrl Pts',(22.817839892186,183.502028447915,-45.2081708191727));
#12924=CARTESIAN_POINT('Ctrl Pts',(29.2444941385794,183.002028447915,-40.5762979824596));
#12925=CARTESIAN_POINT('Ctrl Pts',(35.6711483849729,182.502028447915,-35.9444251457465));
#12926=CARTESIAN_POINT('Ctrl Pts',(40.3519323616533,182.002028447915,-29.5533069226325));
#12927=CARTESIAN_POINT('Ctrl Pts',(45.0327163383337,181.502028447915,-23.1621886995185));
#12928=CARTESIAN_POINT('Ctrl Pts',(47.5094422967239,181.002028447915,-15.6374322712211));
#12929=CARTESIAN_POINT('Ctrl Pts',(49.9861682551141,180.502028447915,-8.11267584292359));
#12930=CARTESIAN_POINT('Ctrl Pts',(50.0163970020424,180.002028447915,-0.190856796705295));
#12931=CARTESIAN_POINT('Ctrl Pts',(50.0466257489707,179.502028447915,7.730962249513));
#12932=CARTESIAN_POINT('Ctrl Pts',(47.6273982840717,179.002028447915,15.2744010708495));
#12933=CARTESIAN_POINT('Ctrl Pts',(45.2081708191727,178.502028447915,22.817839892186));
#12934=CARTESIAN_POINT('Ctrl Pts',(40.5762979824596,178.002028447915,29.2444941385794));
#12935=CARTESIAN_POINT('Ctrl Pts',(35.9444251457465,177.502028447915,35.6711483849729));
#12936=CARTESIAN_POINT('Ctrl Pts',(29.5533069226325,177.002028447915,40.3519323616533));
#12937=CARTESIAN_POINT('Ctrl Pts',(23.1621886995185,176.502028447915,45.0327163383337));
#12938=CARTESIAN_POINT('Ctrl Pts',(15.6374322712211,176.002028447915,47.5094422967239));
#12939=CARTESIAN_POINT('Ctrl Pts',(8.11267584292359,175.502028447915,49.9861682551141));
#12940=CARTESIAN_POINT('Ctrl Pts',(0.190856796705285,175.002028447915,50.0163970020424));
#12941=CARTESIAN_POINT('Ctrl Pts',(0.000256710972400879,237.995967593475,
50.0163970020424));
#12942=CARTESIAN_POINT('Ctrl Pts',(-7.92156233524589,237.495967593475,50.0164376610661));
#12943=CARTESIAN_POINT('Ctrl Pts',(-15.4556725243922,236.995967593475,47.5684996184509));
#12944=CARTESIAN_POINT('Ctrl Pts',(-22.9897827135384,236.495967593475,45.1205615758357));
#12945=CARTESIAN_POINT('Ctrl Pts',(-29.3986928470667,235.995967593475,40.4642660629801));
#12946=CARTESIAN_POINT('Ctrl Pts',(-35.8076029805949,235.495967593475,35.8079705501245));
#12947=CARTESIAN_POINT('Ctrl Pts',(-40.4639642811328,234.995967593475,29.3991082141453));
#12948=CARTESIAN_POINT('Ctrl Pts',(-45.1203255816707,234.495967593475,22.990245878166));
#12949=CARTESIAN_POINT('Ctrl Pts',(-47.5683409623447,233.995967593475,15.4561608176784));
#12950=CARTESIAN_POINT('Ctrl Pts',(-50.0163563430187,233.495967593475,7.9220757571907));
#12951=CARTESIAN_POINT('Ctrl Pts',(-50.0163970020424,232.995967593475,0.000256710972403942));
#12952=CARTESIAN_POINT('Ctrl Pts',(-50.0164376610661,232.495967593475,-7.92156233524589));
#12953=CARTESIAN_POINT('Ctrl Pts',(-47.5684996184509,231.995967593475,-15.4556725243922));
#12954=CARTESIAN_POINT('Ctrl Pts',(-45.1205615758357,231.495967593475,-22.9897827135384));
#12955=CARTESIAN_POINT('Ctrl Pts',(-40.4642660629801,230.995967593475,-29.3986928470667));
#12956=CARTESIAN_POINT('Ctrl Pts',(-35.8079705501245,230.495967593475,-35.8076029805949));
#12957=CARTESIAN_POINT('Ctrl Pts',(-29.3991082141453,229.995967593475,-40.4639642811328));
#12958=CARTESIAN_POINT('Ctrl Pts',(-22.9902458781661,229.495967593475,-45.1203255816707));
#12959=CARTESIAN_POINT('Ctrl Pts',(-15.4561608176784,228.995967593475,-47.5683409623447));
#12960=CARTESIAN_POINT('Ctrl Pts',(-7.92207575719071,228.495967593475,-50.0163563430187));
#12961=CARTESIAN_POINT('Ctrl Pts',(-0.000256710972407005,227.995967593475,
-50.0163970020424));
#12962=CARTESIAN_POINT('Ctrl Pts',(7.92156233524589,227.495967593475,-50.0164376610661));
#12963=CARTESIAN_POINT('Ctrl Pts',(15.4556725243922,226.995967593475,-47.5684996184509));
#12964=CARTESIAN_POINT('Ctrl Pts',(22.9897827135384,226.495967593475,-45.1205615758357));
#12965=CARTESIAN_POINT('Ctrl Pts',(29.3986928470667,225.995967593475,-40.4642660629801));
#12966=CARTESIAN_POINT('Ctrl Pts',(35.8076029805949,225.495967593475,-35.8079705501245));
#12967=CARTESIAN_POINT('Ctrl Pts',(40.4639642811328,224.995967593475,-29.3991082141453));
#12968=CARTESIAN_POINT('Ctrl Pts',(45.1203255816707,224.495967593475,-22.9902458781661));
#12969=CARTESIAN_POINT('Ctrl Pts',(47.5683409623447,223.995967593475,-15.4561608176784));
#12970=CARTESIAN_POINT('Ctrl Pts',(50.0163563430187,223.495967593475,-7.92207575719071));
#12971=CARTESIAN_POINT('Ctrl Pts',(50.0163970020424,222.995967593475,-0.000256710972410067));
#12972=CARTESIAN_POINT('Ctrl Pts',(50.0164376610661,222.495967593475,7.92156233524589));
#12973=CARTESIAN_POINT('Ctrl Pts',(47.5684996184509,221.995967593475,15.4556725243922));
#12974=CARTESIAN_POINT('Ctrl Pts',(45.1205615758358,221.495967593475,22.9897827135384));
#12975=CARTESIAN_POINT('Ctrl Pts',(40.4642660629801,220.995967593475,29.3986928470667));
#12976=CARTESIAN_POINT('Ctrl Pts',(35.8079705501245,220.495967593475,35.8076029805949));
#12977=CARTESIAN_POINT('Ctrl Pts',(29.3991082141453,219.995967593475,40.4639642811328));
#12978=CARTESIAN_POINT('Ctrl Pts',(22.9902458781661,219.495967593475,45.1203255816707));
#12979=CARTESIAN_POINT('Ctrl Pts',(15.4561608176784,218.995967593475,47.5683409623447));
#12980=CARTESIAN_POINT('Ctrl Pts',(7.92207575719071,218.495967593475,50.0163563430187));
#12981=CARTESIAN_POINT('Ctrl Pts',(0.000256710972400879,217.995967593475,
50.0163970020424));
#12982=CARTESIAN_POINT('Ctrl Pts',(-7.92156233524589,217.495967593475,50.0164376610661));
#12983=CARTESIAN_POINT('Ctrl Pts',(-15.4556725243922,216.995967593475,47.5684996184509));
#12984=CARTESIAN_POINT('Ctrl Pts',(-22.9897827135384,216.495967593475,45.1205615758357));
#12985=CARTESIAN_POINT('Ctrl Pts',(-29.3986928470667,215.995967593475,40.4642660629801));
#12986=CARTESIAN_POINT('Ctrl Pts',(-35.8076029805949,215.495967593475,35.8079705501245));
#12987=CARTESIAN_POINT('Ctrl Pts',(-40.4639642811328,214.995967593475,29.3991082141453));
#12988=CARTESIAN_POINT('Ctrl Pts',(-45.1203255816707,214.495967593475,22.990245878166));
#12989=CARTESIAN_POINT('Ctrl Pts',(-47.5683409623447,213.995967593475,15.4561608176784));
#12990=CARTESIAN_POINT('Ctrl Pts',(-50.0163563430187,213.495967593475,7.9220757571907));
#12991=CARTESIAN_POINT('Ctrl Pts',(-50.0163970020424,212.995967593475,0.000256710972403942));
#12992=CARTESIAN_POINT('Ctrl Pts',(-50.0164376610661,212.495967593475,-7.92156233524589));
#12993=CARTESIAN_POINT('Ctrl Pts',(-47.5684996184509,211.995967593475,-15.4556725243922));
#12994=CARTESIAN_POINT('Ctrl Pts',(-45.1205615758357,211.495967593475,-22.9897827135384));
#12995=CARTESIAN_POINT('Ctrl Pts',(-40.4642660629801,210.995967593475,-29.3986928470667));
#12996=CARTESIAN_POINT('Ctrl Pts',(-35.8079705501245,210.495967593475,-35.8076029805949));
#12997=CARTESIAN_POINT('Ctrl Pts',(-29.3991082141453,209.995967593475,-40.4639642811328));
#12998=CARTESIAN_POINT('Ctrl Pts',(-22.9902458781661,209.495967593475,-45.1203255816707));
#12999=CARTESIAN_POINT('Ctrl Pts',(-15.4561608176784,208.995967593475,-47.5683409623447));
#13000=CARTESIAN_POINT('Ctrl Pts',(-7.92207575719071,208.495967593475,-50.0163563430187));
#13001=CARTESIAN_POINT('Ctrl Pts',(-0.000256710972407005,207.995967593475,
-50.0163970020424));
#13002=CARTESIAN_POINT('Ctrl Pts',(7.92156233524589,207.495967593475,-50.0164376610661));
#13003=CARTESIAN_POINT('Ctrl Pts',(15.4556725243922,206.995967593475,-47.5684996184509));
#13004=CARTESIAN_POINT('Ctrl Pts',(22.9897827135384,206.495967593475,-45.1205615758357));
#13005=CARTESIAN_POINT('Ctrl Pts',(29.3986928470667,205.995967593475,-40.4642660629801));
#13006=CARTESIAN_POINT('Ctrl Pts',(35.8076029805949,205.495967593475,-35.8079705501245));
#13007=CARTESIAN_POINT('Ctrl Pts',(40.4639642811328,204.995967593475,-29.3991082141453));
#13008=CARTESIAN_POINT('Ctrl Pts',(45.1203255816707,204.495967593475,-22.9902458781661));
#13009=CARTESIAN_POINT('Ctrl Pts',(47.5683409623447,203.995967593475,-15.4561608176784));
#13010=CARTESIAN_POINT('Ctrl Pts',(50.0163563430187,203.495967593475,-7.92207575719071));
#13011=CARTESIAN_POINT('Ctrl Pts',(50.0163970020424,202.995967593475,-0.000256710972410067));
#13012=CARTESIAN_POINT('Ctrl Pts',(50.0164376610661,202.495967593475,7.92156233524589));
#13013=CARTESIAN_POINT('Ctrl Pts',(47.5684996184509,201.995967593475,15.4556725243922));
#13014=CARTESIAN_POINT('Ctrl Pts',(45.1205615758358,201.495967593475,22.9897827135384));
#13015=CARTESIAN_POINT('Ctrl Pts',(40.4642660629801,200.995967593475,29.3986928470667));
#13016=CARTESIAN_POINT('Ctrl Pts',(35.8079705501245,200.495967593475,35.8076029805949));
#13017=CARTESIAN_POINT('Ctrl Pts',(29.3991082141453,199.995967593475,40.4639642811328));
#13018=CARTESIAN_POINT('Ctrl Pts',(22.9902458781661,199.495967593475,45.1203255816707));
#13019=CARTESIAN_POINT('Ctrl Pts',(15.4561608176784,198.995967593475,47.5683409623447));
#13020=CARTESIAN_POINT('Ctrl Pts',(7.92207575719071,198.495967593475,50.0163563430187));
#13021=CARTESIAN_POINT('Ctrl Pts',(0.000256710972400879,197.995967593475,
50.0163970020424));
#13022=CARTESIAN_POINT('Ctrl Pts',(-7.92156233524589,197.495967593475,50.0164376610661));
#13023=CARTESIAN_POINT('Ctrl Pts',(-15.4556725243922,196.995967593475,47.5684996184509));
#13024=CARTESIAN_POINT('Ctrl Pts',(-22.9897827135384,196.495967593475,45.1205615758357));
#13025=CARTESIAN_POINT('Ctrl Pts',(-29.3986928470667,195.995967593475,40.4642660629801));
#13026=CARTESIAN_POINT('Ctrl Pts',(-35.8076029805949,195.495967593475,35.8079705501245));
#13027=CARTESIAN_POINT('Ctrl Pts',(-40.4639642811328,194.995967593475,29.3991082141453));
#13028=CARTESIAN_POINT('Ctrl Pts',(-45.1203255816707,194.495967593475,22.990245878166));
#13029=CARTESIAN_POINT('Ctrl Pts',(-47.5683409623447,193.995967593475,15.4561608176784));
#13030=CARTESIAN_POINT('Ctrl Pts',(-50.0163563430187,193.495967593475,7.9220757571907));
#13031=CARTESIAN_POINT('Ctrl Pts',(-50.0163970020424,192.995967593475,0.000256710972403942));
#13032=CARTESIAN_POINT('Ctrl Pts',(-50.0164376610661,192.495967593475,-7.92156233524589));
#13033=CARTESIAN_POINT('Ctrl Pts',(-47.5684996184509,191.995967593475,-15.4556725243922));
#13034=CARTESIAN_POINT('Ctrl Pts',(-45.1205615758357,191.495967593475,-22.9897827135384));
#13035=CARTESIAN_POINT('Ctrl Pts',(-40.4642660629801,190.995967593475,-29.3986928470667));
#13036=CARTESIAN_POINT('Ctrl Pts',(-35.8079705501245,190.495967593475,-35.8076029805949));
#13037=CARTESIAN_POINT('Ctrl Pts',(-29.3991082141453,189.995967593475,-40.4639642811328));
#13038=CARTESIAN_POINT('Ctrl Pts',(-22.9902458781661,189.495967593475,-45.1203255816707));
#13039=CARTESIAN_POINT('Ctrl Pts',(-15.4561608176784,188.995967593475,-47.5683409623447));
#13040=CARTESIAN_POINT('Ctrl Pts',(-7.92207575719071,188.495967593475,-50.0163563430187));
#13041=CARTESIAN_POINT('Ctrl Pts',(-0.000256710972407005,187.995967593475,
-50.0163970020424));
#13042=CARTESIAN_POINT('Ctrl Pts',(7.92156233524589,187.495967593475,-50.0164376610661));
#13043=CARTESIAN_POINT('Ctrl Pts',(15.4556725243922,186.995967593475,-47.5684996184509));
#13044=CARTESIAN_POINT('Ctrl Pts',(22.9897827135384,186.495967593475,-45.1205615758357));
#13045=CARTESIAN_POINT('Ctrl Pts',(29.3986928470667,185.995967593475,-40.4642660629801));
#13046=CARTESIAN_POINT('Ctrl Pts',(35.8076029805949,185.495967593475,-35.8079705501245));
#13047=CARTESIAN_POINT('Ctrl Pts',(40.4639642811328,184.995967593475,-29.3991082141453));
#13048=CARTESIAN_POINT('Ctrl Pts',(45.1203255816707,184.495967593475,-22.9902458781661));
#13049=CARTESIAN_POINT('Ctrl Pts',(47.5683409623447,183.995967593475,-15.4561608176784));
#13050=CARTESIAN_POINT('Ctrl Pts',(50.0163563430187,183.495967593475,-7.92207575719071));
#13051=CARTESIAN_POINT('Ctrl Pts',(50.0163970020424,182.995967593475,-0.000256710972410067));
#13052=CARTESIAN_POINT('Ctrl Pts',(50.0164376610661,182.495967593475,7.92156233524589));
#13053=CARTESIAN_POINT('Ctrl Pts',(47.5684996184509,181.995967593475,15.4556725243922));
#13054=CARTESIAN_POINT('Ctrl Pts',(45.1205615758358,181.495967593475,22.9897827135384));
#13055=CARTESIAN_POINT('Ctrl Pts',(40.4642660629801,180.995967593475,29.3986928470667));
#13056=CARTESIAN_POINT('Ctrl Pts',(35.8079705501245,180.495967593475,35.8076029805949));
#13057=CARTESIAN_POINT('Ctrl Pts',(29.3991082141453,179.995967593475,40.4639642811328));
#13058=CARTESIAN_POINT('Ctrl Pts',(22.9902458781661,179.495967593475,45.1203255816707));
#13059=CARTESIAN_POINT('Ctrl Pts',(15.4561608176784,178.995967593475,47.5683409623447));
#13060=CARTESIAN_POINT('Ctrl Pts',(7.92207575719071,178.495967593475,50.0163563430187));
#13061=CARTESIAN_POINT('Ctrl Pts',(0.000256710972400879,177.995967593475,
50.0163970020424));
#13062=CARTESIAN_POINT('Ctrl Pts',(0.00025671097240121,237.995967593475,
7.5));
#13063=CARTESIAN_POINT('Ctrl Pts',(-1.18762659146162,237.495967593475,7.50004065902369));
#13064=CARTESIAN_POINT('Ctrl Pts',(-2.317383311169,236.995967593475,7.13300320026677));
#13065=CARTESIAN_POINT('Ctrl Pts',(-3.44714003087638,236.495967593475,6.76596574150984));
#13066=CARTESIAN_POINT('Ctrl Pts',(-4.40818170865423,235.995967593475,6.06777834873578));
#13067=CARTESIAN_POINT('Ctrl Pts',(-5.36922338643209,235.495967593475,5.36959095596173));
#13068=CARTESIAN_POINT('Ctrl Pts',(-6.06747656688843,234.995967593475,4.40859707573286));
#13069=CARTESIAN_POINT('Ctrl Pts',(-6.76572974734476,234.495967593475,3.447603195504));
#13070=CARTESIAN_POINT('Ctrl Pts',(-7.13284454416054,233.995967593475,2.31787160445521));
#13071=CARTESIAN_POINT('Ctrl Pts',(-7.49995934097631,233.495967593475,1.18814001340642));
#13072=CARTESIAN_POINT('Ctrl Pts',(-7.5,232.995967593475,0.000256710972401669));
#13073=CARTESIAN_POINT('Ctrl Pts',(-7.50004065902369,232.495967593475,-1.18762659146162));
#13074=CARTESIAN_POINT('Ctrl Pts',(-7.13300320026677,231.995967593475,-2.317383311169));
#13075=CARTESIAN_POINT('Ctrl Pts',(-6.76596574150984,231.495967593475,-3.44714003087638));
#13076=CARTESIAN_POINT('Ctrl Pts',(-6.06777834873578,230.995967593475,-4.40818170865423));
#13077=CARTESIAN_POINT('Ctrl Pts',(-5.36959095596173,230.495967593475,-5.36922338643209));
#13078=CARTESIAN_POINT('Ctrl Pts',(-4.40859707573286,229.995967593475,-6.06747656688843));
#13079=CARTESIAN_POINT('Ctrl Pts',(-3.447603195504,229.495967593475,-6.76572974734476));
#13080=CARTESIAN_POINT('Ctrl Pts',(-2.31787160445521,228.995967593475,-7.13284454416054));
#13081=CARTESIAN_POINT('Ctrl Pts',(-1.18814001340642,228.495967593475,-7.49995934097631));
#13082=CARTESIAN_POINT('Ctrl Pts',(-0.000256710972402128,227.995967593475,
-7.5));
#13083=CARTESIAN_POINT('Ctrl Pts',(1.18762659146162,227.495967593475,-7.50004065902369));
#13084=CARTESIAN_POINT('Ctrl Pts',(2.317383311169,226.995967593475,-7.13300320026677));
#13085=CARTESIAN_POINT('Ctrl Pts',(3.44714003087638,226.495967593475,-6.76596574150984));
#13086=CARTESIAN_POINT('Ctrl Pts',(4.40818170865423,225.995967593475,-6.06777834873578));
#13087=CARTESIAN_POINT('Ctrl Pts',(5.36922338643209,225.495967593475,-5.36959095596173));
#13088=CARTESIAN_POINT('Ctrl Pts',(6.06747656688843,224.995967593475,-4.40859707573286));
#13089=CARTESIAN_POINT('Ctrl Pts',(6.76572974734476,224.495967593475,-3.447603195504));
#13090=CARTESIAN_POINT('Ctrl Pts',(7.13284454416054,223.995967593475,-2.31787160445521));
#13091=CARTESIAN_POINT('Ctrl Pts',(7.49995934097631,223.495967593475,-1.18814001340642));
#13092=CARTESIAN_POINT('Ctrl Pts',(7.5,222.995967593475,-0.000256710972402588));
#13093=CARTESIAN_POINT('Ctrl Pts',(7.50004065902369,222.495967593475,1.18762659146162));
#13094=CARTESIAN_POINT('Ctrl Pts',(7.13300320026677,221.995967593475,2.317383311169));
#13095=CARTESIAN_POINT('Ctrl Pts',(6.76596574150984,221.495967593475,3.44714003087638));
#13096=CARTESIAN_POINT('Ctrl Pts',(6.06777834873579,220.995967593475,4.40818170865423));
#13097=CARTESIAN_POINT('Ctrl Pts',(5.36959095596173,220.495967593475,5.36922338643209));
#13098=CARTESIAN_POINT('Ctrl Pts',(4.40859707573286,219.995967593475,6.06747656688843));
#13099=CARTESIAN_POINT('Ctrl Pts',(3.447603195504,219.495967593475,6.76572974734476));
#13100=CARTESIAN_POINT('Ctrl Pts',(2.31787160445521,218.995967593475,7.13284454416054));
#13101=CARTESIAN_POINT('Ctrl Pts',(1.18814001340643,218.495967593475,7.49995934097631));
#13102=CARTESIAN_POINT('Ctrl Pts',(0.00025671097240121,217.995967593475,
7.5));
#13103=CARTESIAN_POINT('Ctrl Pts',(-1.18762659146162,217.495967593475,7.50004065902369));
#13104=CARTESIAN_POINT('Ctrl Pts',(-2.317383311169,216.995967593475,7.13300320026677));
#13105=CARTESIAN_POINT('Ctrl Pts',(-3.44714003087638,216.495967593475,6.76596574150984));
#13106=CARTESIAN_POINT('Ctrl Pts',(-4.40818170865423,215.995967593475,6.06777834873578));
#13107=CARTESIAN_POINT('Ctrl Pts',(-5.36922338643209,215.495967593475,5.36959095596173));
#13108=CARTESIAN_POINT('Ctrl Pts',(-6.06747656688843,214.995967593475,4.40859707573286));
#13109=CARTESIAN_POINT('Ctrl Pts',(-6.76572974734476,214.495967593475,3.447603195504));
#13110=CARTESIAN_POINT('Ctrl Pts',(-7.13284454416054,213.995967593475,2.31787160445521));
#13111=CARTESIAN_POINT('Ctrl Pts',(-7.49995934097631,213.495967593475,1.18814001340642));
#13112=CARTESIAN_POINT('Ctrl Pts',(-7.5,212.995967593475,0.000256710972401669));
#13113=CARTESIAN_POINT('Ctrl Pts',(-7.50004065902369,212.495967593475,-1.18762659146162));
#13114=CARTESIAN_POINT('Ctrl Pts',(-7.13300320026677,211.995967593475,-2.317383311169));
#13115=CARTESIAN_POINT('Ctrl Pts',(-6.76596574150984,211.495967593475,-3.44714003087638));
#13116=CARTESIAN_POINT('Ctrl Pts',(-6.06777834873578,210.995967593475,-4.40818170865423));
#13117=CARTESIAN_POINT('Ctrl Pts',(-5.36959095596173,210.495967593475,-5.36922338643209));
#13118=CARTESIAN_POINT('Ctrl Pts',(-4.40859707573286,209.995967593475,-6.06747656688843));
#13119=CARTESIAN_POINT('Ctrl Pts',(-3.447603195504,209.495967593475,-6.76572974734476));
#13120=CARTESIAN_POINT('Ctrl Pts',(-2.31787160445521,208.995967593475,-7.13284454416054));
#13121=CARTESIAN_POINT('Ctrl Pts',(-1.18814001340642,208.495967593475,-7.49995934097631));
#13122=CARTESIAN_POINT('Ctrl Pts',(-0.000256710972402128,207.995967593475,
-7.5));
#13123=CARTESIAN_POINT('Ctrl Pts',(1.18762659146162,207.495967593475,-7.50004065902369));
#13124=CARTESIAN_POINT('Ctrl Pts',(2.317383311169,206.995967593475,-7.13300320026677));
#13125=CARTESIAN_POINT('Ctrl Pts',(3.44714003087638,206.495967593475,-6.76596574150984));
#13126=CARTESIAN_POINT('Ctrl Pts',(4.40818170865423,205.995967593475,-6.06777834873578));
#13127=CARTESIAN_POINT('Ctrl Pts',(5.36922338643209,205.495967593475,-5.36959095596173));
#13128=CARTESIAN_POINT('Ctrl Pts',(6.06747656688843,204.995967593475,-4.40859707573286));
#13129=CARTESIAN_POINT('Ctrl Pts',(6.76572974734476,204.495967593475,-3.447603195504));
#13130=CARTESIAN_POINT('Ctrl Pts',(7.13284454416054,203.995967593475,-2.31787160445521));
#13131=CARTESIAN_POINT('Ctrl Pts',(7.49995934097631,203.495967593475,-1.18814001340642));
#13132=CARTESIAN_POINT('Ctrl Pts',(7.5,202.995967593475,-0.000256710972402588));
#13133=CARTESIAN_POINT('Ctrl Pts',(7.50004065902369,202.495967593475,1.18762659146162));
#13134=CARTESIAN_POINT('Ctrl Pts',(7.13300320026677,201.995967593475,2.317383311169));
#13135=CARTESIAN_POINT('Ctrl Pts',(6.76596574150984,201.495967593475,3.44714003087638));
#13136=CARTESIAN_POINT('Ctrl Pts',(6.06777834873579,200.995967593475,4.40818170865423));
#13137=CARTESIAN_POINT('Ctrl Pts',(5.36959095596173,200.495967593475,5.36922338643209));
#13138=CARTESIAN_POINT('Ctrl Pts',(4.40859707573286,199.995967593475,6.06747656688843));
#13139=CARTESIAN_POINT('Ctrl Pts',(3.447603195504,199.495967593475,6.76572974734476));
#13140=CARTESIAN_POINT('Ctrl Pts',(2.31787160445521,198.995967593475,7.13284454416054));
#13141=CARTESIAN_POINT('Ctrl Pts',(1.18814001340643,198.495967593475,7.49995934097631));
#13142=CARTESIAN_POINT('Ctrl Pts',(0.00025671097240121,197.995967593475,
7.5));
#13143=CARTESIAN_POINT('Ctrl Pts',(-1.18762659146162,197.495967593475,7.50004065902369));
#13144=CARTESIAN_POINT('Ctrl Pts',(-2.317383311169,196.995967593475,7.13300320026677));
#13145=CARTESIAN_POINT('Ctrl Pts',(-3.44714003087638,196.495967593475,6.76596574150984));
#13146=CARTESIAN_POINT('Ctrl Pts',(-4.40818170865423,195.995967593475,6.06777834873578));
#13147=CARTESIAN_POINT('Ctrl Pts',(-5.36922338643209,195.495967593475,5.36959095596173));
#13148=CARTESIAN_POINT('Ctrl Pts',(-6.06747656688843,194.995967593475,4.40859707573286));
#13149=CARTESIAN_POINT('Ctrl Pts',(-6.76572974734476,194.495967593475,3.447603195504));
#13150=CARTESIAN_POINT('Ctrl Pts',(-7.13284454416054,193.995967593475,2.31787160445521));
#13151=CARTESIAN_POINT('Ctrl Pts',(-7.49995934097631,193.495967593475,1.18814001340642));
#13152=CARTESIAN_POINT('Ctrl Pts',(-7.5,192.995967593475,0.000256710972401669));
#13153=CARTESIAN_POINT('Ctrl Pts',(-7.50004065902369,192.495967593475,-1.18762659146162));
#13154=CARTESIAN_POINT('Ctrl Pts',(-7.13300320026677,191.995967593475,-2.317383311169));
#13155=CARTESIAN_POINT('Ctrl Pts',(-6.76596574150984,191.495967593475,-3.44714003087638));
#13156=CARTESIAN_POINT('Ctrl Pts',(-6.06777834873578,190.995967593475,-4.40818170865423));
#13157=CARTESIAN_POINT('Ctrl Pts',(-5.36959095596173,190.495967593475,-5.36922338643209));
#13158=CARTESIAN_POINT('Ctrl Pts',(-4.40859707573286,189.995967593475,-6.06747656688843));
#13159=CARTESIAN_POINT('Ctrl Pts',(-3.447603195504,189.495967593475,-6.76572974734476));
#13160=CARTESIAN_POINT('Ctrl Pts',(-2.31787160445521,188.995967593475,-7.13284454416054));
#13161=CARTESIAN_POINT('Ctrl Pts',(-1.18814001340642,188.495967593475,-7.49995934097631));
#13162=CARTESIAN_POINT('Ctrl Pts',(-0.000256710972402128,187.995967593475,
-7.5));
#13163=CARTESIAN_POINT('Ctrl Pts',(1.18762659146162,187.495967593475,-7.50004065902369));
#13164=CARTESIAN_POINT('Ctrl Pts',(2.317383311169,186.995967593475,-7.13300320026677));
#13165=CARTESIAN_POINT('Ctrl Pts',(3.44714003087638,186.495967593475,-6.76596574150984));
#13166=CARTESIAN_POINT('Ctrl Pts',(4.40818170865423,185.995967593475,-6.06777834873578));
#13167=CARTESIAN_POINT('Ctrl Pts',(5.36922338643209,185.495967593475,-5.36959095596173));
#13168=CARTESIAN_POINT('Ctrl Pts',(6.06747656688843,184.995967593475,-4.40859707573286));
#13169=CARTESIAN_POINT('Ctrl Pts',(6.76572974734476,184.495967593475,-3.447603195504));
#13170=CARTESIAN_POINT('Ctrl Pts',(7.13284454416054,183.995967593475,-2.31787160445521));
#13171=CARTESIAN_POINT('Ctrl Pts',(7.49995934097631,183.495967593475,-1.18814001340642));
#13172=CARTESIAN_POINT('Ctrl Pts',(7.5,182.995967593475,-0.000256710972402588));
#13173=CARTESIAN_POINT('Ctrl Pts',(7.50004065902369,182.495967593475,1.18762659146162));
#13174=CARTESIAN_POINT('Ctrl Pts',(7.13300320026677,181.995967593475,2.317383311169));
#13175=CARTESIAN_POINT('Ctrl Pts',(6.76596574150984,181.495967593475,3.44714003087638));
#13176=CARTESIAN_POINT('Ctrl Pts',(6.06777834873579,180.995967593475,4.40818170865423));
#13177=CARTESIAN_POINT('Ctrl Pts',(5.36959095596173,180.495967593475,5.36922338643209));
#13178=CARTESIAN_POINT('Ctrl Pts',(4.40859707573286,179.995967593475,6.06747656688843));
#13179=CARTESIAN_POINT('Ctrl Pts',(3.447603195504,179.495967593475,6.76572974734476));
#13180=CARTESIAN_POINT('Ctrl Pts',(2.31787160445521,178.995967593475,7.13284454416054));
#13181=CARTESIAN_POINT('Ctrl Pts',(1.18814001340643,178.495967593475,7.49995934097631));
#13182=CARTESIAN_POINT('Ctrl Pts',(0.00025671097240121,177.995967593475,
7.5));
#13183=CARTESIAN_POINT('Ctrl Pts',(0.000256710972400845,237.995967593475,
50.0163970020424));
#13184=CARTESIAN_POINT('Ctrl Pts',(-7.92156233524589,237.495967593475,50.0164376610661));
#13185=CARTESIAN_POINT('Ctrl Pts',(-15.4556725243922,236.995967593475,47.5684996184509));
#13186=CARTESIAN_POINT('Ctrl Pts',(-22.9897827135384,236.495967593475,45.1205615758357));
#13187=CARTESIAN_POINT('Ctrl Pts',(-29.3986928470667,235.995967593475,40.4642660629801));
#13188=CARTESIAN_POINT('Ctrl Pts',(-35.8076029805949,235.495967593475,35.8079705501245));
#13189=CARTESIAN_POINT('Ctrl Pts',(-40.4639642811328,234.995967593475,29.3991082141453));
#13190=CARTESIAN_POINT('Ctrl Pts',(-45.1203255816707,234.495967593475,22.990245878166));
#13191=CARTESIAN_POINT('Ctrl Pts',(-47.5683409623447,233.995967593475,15.4561608176784));
#13192=CARTESIAN_POINT('Ctrl Pts',(-50.0163563430187,233.495967593475,7.9220757571907));
#13193=CARTESIAN_POINT('Ctrl Pts',(-50.0163970020424,232.995967593475,0.000256710972403907));
#13194=CARTESIAN_POINT('Ctrl Pts',(-50.0164376610661,232.495967593475,-7.92156233524589));
#13195=CARTESIAN_POINT('Ctrl Pts',(-47.5684996184509,231.995967593475,-15.4556725243922));
#13196=CARTESIAN_POINT('Ctrl Pts',(-45.1205615758357,231.495967593475,-22.9897827135384));
#13197=CARTESIAN_POINT('Ctrl Pts',(-40.4642660629801,230.995967593475,-29.3986928470667));
#13198=CARTESIAN_POINT('Ctrl Pts',(-35.8079705501245,230.495967593475,-35.8076029805949));
#13199=CARTESIAN_POINT('Ctrl Pts',(-29.3991082141453,229.995967593475,-40.4639642811328));
#13200=CARTESIAN_POINT('Ctrl Pts',(-22.9902458781661,229.495967593475,-45.1203255816707));
#13201=CARTESIAN_POINT('Ctrl Pts',(-15.4561608176784,228.995967593475,-47.5683409623447));
#13202=CARTESIAN_POINT('Ctrl Pts',(-7.92207575719071,228.495967593475,-50.0163563430187));
#13203=CARTESIAN_POINT('Ctrl Pts',(-0.00025671097240697,227.995967593475,
-50.0163970020424));
#13204=CARTESIAN_POINT('Ctrl Pts',(7.92156233524589,227.495967593475,-50.0164376610661));
#13205=CARTESIAN_POINT('Ctrl Pts',(15.4556725243922,226.995967593475,-47.5684996184509));
#13206=CARTESIAN_POINT('Ctrl Pts',(22.9897827135384,226.495967593475,-45.1205615758357));
#13207=CARTESIAN_POINT('Ctrl Pts',(29.3986928470667,225.995967593475,-40.4642660629801));
#13208=CARTESIAN_POINT('Ctrl Pts',(35.8076029805949,225.495967593475,-35.8079705501245));
#13209=CARTESIAN_POINT('Ctrl Pts',(40.4639642811328,224.995967593475,-29.3991082141453));
#13210=CARTESIAN_POINT('Ctrl Pts',(45.1203255816707,224.495967593475,-22.9902458781661));
#13211=CARTESIAN_POINT('Ctrl Pts',(47.5683409623447,223.995967593475,-15.4561608176784));
#13212=CARTESIAN_POINT('Ctrl Pts',(50.0163563430187,223.495967593475,-7.92207575719071));
#13213=CARTESIAN_POINT('Ctrl Pts',(50.0163970020424,222.995967593475,-0.000256710972410033));
#13214=CARTESIAN_POINT('Ctrl Pts',(50.0164376610661,222.495967593475,7.92156233524589));
#13215=CARTESIAN_POINT('Ctrl Pts',(47.5684996184509,221.995967593475,15.4556725243922));
#13216=CARTESIAN_POINT('Ctrl Pts',(45.1205615758358,221.495967593475,22.9897827135384));
#13217=CARTESIAN_POINT('Ctrl Pts',(40.4642660629801,220.995967593475,29.3986928470667));
#13218=CARTESIAN_POINT('Ctrl Pts',(35.8079705501245,220.495967593475,35.8076029805949));
#13219=CARTESIAN_POINT('Ctrl Pts',(29.3991082141453,219.995967593475,40.4639642811328));
#13220=CARTESIAN_POINT('Ctrl Pts',(22.9902458781661,219.495967593475,45.1203255816707));
#13221=CARTESIAN_POINT('Ctrl Pts',(15.4561608176784,218.995967593475,47.5683409623447));
#13222=CARTESIAN_POINT('Ctrl Pts',(7.92207575719071,218.495967593475,50.0163563430187));
#13223=CARTESIAN_POINT('Ctrl Pts',(0.000256710972400845,217.995967593475,
50.0163970020424));
#13224=CARTESIAN_POINT('Ctrl Pts',(-7.92156233524589,217.495967593475,50.0164376610661));
#13225=CARTESIAN_POINT('Ctrl Pts',(-15.4556725243922,216.995967593475,47.5684996184509));
#13226=CARTESIAN_POINT('Ctrl Pts',(-22.9897827135384,216.495967593475,45.1205615758357));
#13227=CARTESIAN_POINT('Ctrl Pts',(-29.3986928470667,215.995967593475,40.4642660629801));
#13228=CARTESIAN_POINT('Ctrl Pts',(-35.8076029805949,215.495967593475,35.8079705501245));
#13229=CARTESIAN_POINT('Ctrl Pts',(-40.4639642811328,214.995967593475,29.3991082141453));
#13230=CARTESIAN_POINT('Ctrl Pts',(-45.1203255816707,214.495967593475,22.990245878166));
#13231=CARTESIAN_POINT('Ctrl Pts',(-47.5683409623447,213.995967593475,15.4561608176784));
#13232=CARTESIAN_POINT('Ctrl Pts',(-50.0163563430187,213.495967593475,7.9220757571907));
#13233=CARTESIAN_POINT('Ctrl Pts',(-50.0163970020424,212.995967593475,0.000256710972403907));
#13234=CARTESIAN_POINT('Ctrl Pts',(-50.0164376610661,212.495967593475,-7.92156233524589));
#13235=CARTESIAN_POINT('Ctrl Pts',(-47.5684996184509,211.995967593475,-15.4556725243922));
#13236=CARTESIAN_POINT('Ctrl Pts',(-45.1205615758357,211.495967593475,-22.9897827135384));
#13237=CARTESIAN_POINT('Ctrl Pts',(-40.4642660629801,210.995967593475,-29.3986928470667));
#13238=CARTESIAN_POINT('Ctrl Pts',(-35.8079705501245,210.495967593475,-35.8076029805949));
#13239=CARTESIAN_POINT('Ctrl Pts',(-29.3991082141453,209.995967593475,-40.4639642811328));
#13240=CARTESIAN_POINT('Ctrl Pts',(-22.9902458781661,209.495967593475,-45.1203255816707));
#13241=CARTESIAN_POINT('Ctrl Pts',(-15.4561608176784,208.995967593475,-47.5683409623447));
#13242=CARTESIAN_POINT('Ctrl Pts',(-7.92207575719071,208.495967593475,-50.0163563430187));
#13243=CARTESIAN_POINT('Ctrl Pts',(-0.00025671097240697,207.995967593475,
-50.0163970020424));
#13244=CARTESIAN_POINT('Ctrl Pts',(7.92156233524589,207.495967593475,-50.0164376610661));
#13245=CARTESIAN_POINT('Ctrl Pts',(15.4556725243922,206.995967593475,-47.5684996184509));
#13246=CARTESIAN_POINT('Ctrl Pts',(22.9897827135384,206.495967593475,-45.1205615758357));
#13247=CARTESIAN_POINT('Ctrl Pts',(29.3986928470667,205.995967593475,-40.4642660629801));
#13248=CARTESIAN_POINT('Ctrl Pts',(35.8076029805949,205.495967593475,-35.8079705501245));
#13249=CARTESIAN_POINT('Ctrl Pts',(40.4639642811328,204.995967593475,-29.3991082141453));
#13250=CARTESIAN_POINT('Ctrl Pts',(45.1203255816707,204.495967593475,-22.9902458781661));
#13251=CARTESIAN_POINT('Ctrl Pts',(47.5683409623447,203.995967593475,-15.4561608176784));
#13252=CARTESIAN_POINT('Ctrl Pts',(50.0163563430187,203.495967593475,-7.92207575719071));
#13253=CARTESIAN_POINT('Ctrl Pts',(50.0163970020424,202.995967593475,-0.000256710972410033));
#13254=CARTESIAN_POINT('Ctrl Pts',(50.0164376610661,202.495967593475,7.92156233524589));
#13255=CARTESIAN_POINT('Ctrl Pts',(47.5684996184509,201.995967593475,15.4556725243922));
#13256=CARTESIAN_POINT('Ctrl Pts',(45.1205615758358,201.495967593475,22.9897827135384));
#13257=CARTESIAN_POINT('Ctrl Pts',(40.4642660629801,200.995967593475,29.3986928470667));
#13258=CARTESIAN_POINT('Ctrl Pts',(35.8079705501245,200.495967593475,35.8076029805949));
#13259=CARTESIAN_POINT('Ctrl Pts',(29.3991082141453,199.995967593475,40.4639642811328));
#13260=CARTESIAN_POINT('Ctrl Pts',(22.9902458781661,199.495967593475,45.1203255816707));
#13261=CARTESIAN_POINT('Ctrl Pts',(15.4561608176784,198.995967593475,47.5683409623447));
#13262=CARTESIAN_POINT('Ctrl Pts',(7.92207575719071,198.495967593475,50.0163563430187));
#13263=CARTESIAN_POINT('Ctrl Pts',(0.000256710972400845,197.995967593475,
50.0163970020424));
#13264=CARTESIAN_POINT('Ctrl Pts',(-7.92156233524589,197.495967593475,50.0164376610661));
#13265=CARTESIAN_POINT('Ctrl Pts',(-15.4556725243922,196.995967593475,47.5684996184509));
#13266=CARTESIAN_POINT('Ctrl Pts',(-22.9897827135384,196.495967593475,45.1205615758357));
#13267=CARTESIAN_POINT('Ctrl Pts',(-29.3986928470667,195.995967593475,40.4642660629801));
#13268=CARTESIAN_POINT('Ctrl Pts',(-35.8076029805949,195.495967593475,35.8079705501245));
#13269=CARTESIAN_POINT('Ctrl Pts',(-40.4639642811328,194.995967593475,29.3991082141453));
#13270=CARTESIAN_POINT('Ctrl Pts',(-45.1203255816707,194.495967593475,22.990245878166));
#13271=CARTESIAN_POINT('Ctrl Pts',(-47.5683409623447,193.995967593475,15.4561608176784));
#13272=CARTESIAN_POINT('Ctrl Pts',(-50.0163563430187,193.495967593475,7.9220757571907));
#13273=CARTESIAN_POINT('Ctrl Pts',(-50.0163970020424,192.995967593475,0.000256710972403907));
#13274=CARTESIAN_POINT('Ctrl Pts',(-50.0164376610661,192.495967593475,-7.92156233524589));
#13275=CARTESIAN_POINT('Ctrl Pts',(-47.5684996184509,191.995967593475,-15.4556725243922));
#13276=CARTESIAN_POINT('Ctrl Pts',(-45.1205615758357,191.495967593475,-22.9897827135384));
#13277=CARTESIAN_POINT('Ctrl Pts',(-40.4642660629801,190.995967593475,-29.3986928470667));
#13278=CARTESIAN_POINT('Ctrl Pts',(-35.8079705501245,190.495967593475,-35.8076029805949));
#13279=CARTESIAN_POINT('Ctrl Pts',(-29.3991082141453,189.995967593475,-40.4639642811328));
#13280=CARTESIAN_POINT('Ctrl Pts',(-22.9902458781661,189.495967593475,-45.1203255816707));
#13281=CARTESIAN_POINT('Ctrl Pts',(-15.4561608176784,188.995967593475,-47.5683409623447));
#13282=CARTESIAN_POINT('Ctrl Pts',(-7.92207575719071,188.495967593475,-50.0163563430187));
#13283=CARTESIAN_POINT('Ctrl Pts',(-0.00025671097240697,187.995967593475,
-50.0163970020424));
#13284=CARTESIAN_POINT('Ctrl Pts',(7.92156233524589,187.495967593475,-50.0164376610661));
#13285=CARTESIAN_POINT('Ctrl Pts',(15.4556725243922,186.995967593475,-47.5684996184509));
#13286=CARTESIAN_POINT('Ctrl Pts',(22.9897827135384,186.495967593475,-45.1205615758357));
#13287=CARTESIAN_POINT('Ctrl Pts',(29.3986928470667,185.995967593475,-40.4642660629801));
#13288=CARTESIAN_POINT('Ctrl Pts',(35.8076029805949,185.495967593475,-35.8079705501245));
#13289=CARTESIAN_POINT('Ctrl Pts',(40.4639642811328,184.995967593475,-29.3991082141453));
#13290=CARTESIAN_POINT('Ctrl Pts',(45.1203255816707,184.495967593475,-22.9902458781661));
#13291=CARTESIAN_POINT('Ctrl Pts',(47.5683409623447,183.995967593475,-15.4561608176784));
#13292=CARTESIAN_POINT('Ctrl Pts',(50.0163563430187,183.495967593475,-7.92207575719071));
#13293=CARTESIAN_POINT('Ctrl Pts',(50.0163970020424,182.995967593475,-0.000256710972410033));
#13294=CARTESIAN_POINT('Ctrl Pts',(50.0164376610661,182.495967593475,7.92156233524589));
#13295=CARTESIAN_POINT('Ctrl Pts',(47.5684996184509,181.995967593475,15.4556725243922));
#13296=CARTESIAN_POINT('Ctrl Pts',(45.1205615758358,181.495967593475,22.9897827135384));
#13297=CARTESIAN_POINT('Ctrl Pts',(40.4642660629801,180.995967593475,29.3986928470667));
#13298=CARTESIAN_POINT('Ctrl Pts',(35.8079705501245,180.495967593475,35.8076029805949));
#13299=CARTESIAN_POINT('Ctrl Pts',(29.3991082141453,179.995967593475,40.4639642811328));
#13300=CARTESIAN_POINT('Ctrl Pts',(22.9902458781661,179.495967593475,45.1203255816707));
#13301=CARTESIAN_POINT('Ctrl Pts',(15.4561608176784,178.995967593475,47.5683409623447));
#13302=CARTESIAN_POINT('Ctrl Pts',(7.92207575719071,178.495967593475,50.0163563430187));
#13303=CARTESIAN_POINT('Ctrl Pts',(0.000256710972400845,177.995967593475,
50.0163970020424));
#13304=CARTESIAN_POINT('Ctrl Pts',(0.190856796705285,235.002028447915,50.0163970020424));
#13305=CARTESIAN_POINT('Ctrl Pts',(-7.73096224951301,234.502028447915,50.0466257489707));
#13306=CARTESIAN_POINT('Ctrl Pts',(-15.2744010708495,234.002028447915,47.6273982840717));
#13307=CARTESIAN_POINT('Ctrl Pts',(-22.817839892186,233.502028447915,45.2081708191727));
#13308=CARTESIAN_POINT('Ctrl Pts',(-29.2444941385794,233.002028447915,40.5762979824596));
#13309=CARTESIAN_POINT('Ctrl Pts',(-35.6711483849729,232.502028447915,35.9444251457465));
#13310=CARTESIAN_POINT('Ctrl Pts',(-40.3519323616533,232.002028447915,29.5533069226325));
#13311=CARTESIAN_POINT('Ctrl Pts',(-45.0327163383337,231.502028447915,23.1621886995185));
#13312=CARTESIAN_POINT('Ctrl Pts',(-47.5094422967239,231.002028447915,15.6374322712211));
#13313=CARTESIAN_POINT('Ctrl Pts',(-49.9861682551141,230.502028447915,8.11267584292358));
#13314=CARTESIAN_POINT('Ctrl Pts',(-50.0163970020424,230.002028447915,0.190856796705288));
#13315=CARTESIAN_POINT('Ctrl Pts',(-50.0466257489707,229.502028447915,-7.73096224951301));
#13316=CARTESIAN_POINT('Ctrl Pts',(-47.6273982840717,229.002028447915,-15.2744010708495));
#13317=CARTESIAN_POINT('Ctrl Pts',(-45.2081708191727,228.502028447915,-22.817839892186));
#13318=CARTESIAN_POINT('Ctrl Pts',(-40.5762979824596,228.002028447915,-29.2444941385794));
#13319=CARTESIAN_POINT('Ctrl Pts',(-35.9444251457465,227.502028447915,-35.6711483849729));
#13320=CARTESIAN_POINT('Ctrl Pts',(-29.5533069226325,227.002028447915,-40.3519323616533));
#13321=CARTESIAN_POINT('Ctrl Pts',(-23.1621886995185,226.502028447915,-45.0327163383337));
#13322=CARTESIAN_POINT('Ctrl Pts',(-15.6374322712211,226.002028447915,-47.5094422967239));
#13323=CARTESIAN_POINT('Ctrl Pts',(-8.11267584292359,225.502028447915,-49.9861682551141));
#13324=CARTESIAN_POINT('Ctrl Pts',(-0.190856796705292,225.002028447915,
-50.0163970020424));
#13325=CARTESIAN_POINT('Ctrl Pts',(7.730962249513,224.502028447915,-50.0466257489707));
#13326=CARTESIAN_POINT('Ctrl Pts',(15.2744010708495,224.002028447915,-47.6273982840717));
#13327=CARTESIAN_POINT('Ctrl Pts',(22.817839892186,223.502028447915,-45.2081708191727));
#13328=CARTESIAN_POINT('Ctrl Pts',(29.2444941385794,223.002028447915,-40.5762979824596));
#13329=CARTESIAN_POINT('Ctrl Pts',(35.6711483849729,222.502028447915,-35.9444251457465));
#13330=CARTESIAN_POINT('Ctrl Pts',(40.3519323616533,222.002028447915,-29.5533069226325));
#13331=CARTESIAN_POINT('Ctrl Pts',(45.0327163383337,221.502028447915,-23.1621886995185));
#13332=CARTESIAN_POINT('Ctrl Pts',(47.5094422967239,221.002028447915,-15.6374322712211));
#13333=CARTESIAN_POINT('Ctrl Pts',(49.9861682551141,220.502028447915,-8.11267584292359));
#13334=CARTESIAN_POINT('Ctrl Pts',(50.0163970020424,220.002028447915,-0.190856796705295));
#13335=CARTESIAN_POINT('Ctrl Pts',(50.0466257489707,219.502028447915,7.730962249513));
#13336=CARTESIAN_POINT('Ctrl Pts',(47.6273982840717,219.002028447915,15.2744010708495));
#13337=CARTESIAN_POINT('Ctrl Pts',(45.2081708191727,218.502028447915,22.817839892186));
#13338=CARTESIAN_POINT('Ctrl Pts',(40.5762979824596,218.002028447915,29.2444941385794));
#13339=CARTESIAN_POINT('Ctrl Pts',(35.9444251457465,217.502028447915,35.6711483849729));
#13340=CARTESIAN_POINT('Ctrl Pts',(29.5533069226325,217.002028447915,40.3519323616533));
#13341=CARTESIAN_POINT('Ctrl Pts',(23.1621886995185,216.502028447915,45.0327163383337));
#13342=CARTESIAN_POINT('Ctrl Pts',(15.6374322712211,216.002028447915,47.5094422967239));
#13343=CARTESIAN_POINT('Ctrl Pts',(8.11267584292359,215.502028447915,49.9861682551141));
#13344=CARTESIAN_POINT('Ctrl Pts',(0.190856796705285,215.002028447915,50.0163970020424));
#13345=CARTESIAN_POINT('Ctrl Pts',(-7.73096224951301,214.502028447915,50.0466257489707));
#13346=CARTESIAN_POINT('Ctrl Pts',(-15.2744010708495,214.002028447915,47.6273982840717));
#13347=CARTESIAN_POINT('Ctrl Pts',(-22.817839892186,213.502028447915,45.2081708191727));
#13348=CARTESIAN_POINT('Ctrl Pts',(-29.2444941385794,213.002028447915,40.5762979824596));
#13349=CARTESIAN_POINT('Ctrl Pts',(-35.6711483849729,212.502028447915,35.9444251457465));
#13350=CARTESIAN_POINT('Ctrl Pts',(-40.3519323616533,212.002028447915,29.5533069226325));
#13351=CARTESIAN_POINT('Ctrl Pts',(-45.0327163383337,211.502028447915,23.1621886995185));
#13352=CARTESIAN_POINT('Ctrl Pts',(-47.5094422967239,211.002028447915,15.6374322712211));
#13353=CARTESIAN_POINT('Ctrl Pts',(-49.9861682551141,210.502028447915,8.11267584292358));
#13354=CARTESIAN_POINT('Ctrl Pts',(-50.0163970020424,210.002028447915,0.190856796705288));
#13355=CARTESIAN_POINT('Ctrl Pts',(-50.0466257489707,209.502028447915,-7.73096224951301));
#13356=CARTESIAN_POINT('Ctrl Pts',(-47.6273982840717,209.002028447915,-15.2744010708495));
#13357=CARTESIAN_POINT('Ctrl Pts',(-45.2081708191727,208.502028447915,-22.817839892186));
#13358=CARTESIAN_POINT('Ctrl Pts',(-40.5762979824596,208.002028447915,-29.2444941385794));
#13359=CARTESIAN_POINT('Ctrl Pts',(-35.9444251457465,207.502028447915,-35.6711483849729));
#13360=CARTESIAN_POINT('Ctrl Pts',(-29.5533069226325,207.002028447915,-40.3519323616533));
#13361=CARTESIAN_POINT('Ctrl Pts',(-23.1621886995185,206.502028447915,-45.0327163383337));
#13362=CARTESIAN_POINT('Ctrl Pts',(-15.6374322712211,206.002028447915,-47.5094422967239));
#13363=CARTESIAN_POINT('Ctrl Pts',(-8.11267584292359,205.502028447915,-49.9861682551141));
#13364=CARTESIAN_POINT('Ctrl Pts',(-0.190856796705292,205.002028447915,
-50.0163970020424));
#13365=CARTESIAN_POINT('Ctrl Pts',(7.730962249513,204.502028447915,-50.0466257489707));
#13366=CARTESIAN_POINT('Ctrl Pts',(15.2744010708495,204.002028447915,-47.6273982840717));
#13367=CARTESIAN_POINT('Ctrl Pts',(22.817839892186,203.502028447915,-45.2081708191727));
#13368=CARTESIAN_POINT('Ctrl Pts',(29.2444941385794,203.002028447915,-40.5762979824596));
#13369=CARTESIAN_POINT('Ctrl Pts',(35.6711483849729,202.502028447915,-35.9444251457465));
#13370=CARTESIAN_POINT('Ctrl Pts',(40.3519323616533,202.002028447915,-29.5533069226325));
#13371=CARTESIAN_POINT('Ctrl Pts',(45.0327163383337,201.502028447915,-23.1621886995185));
#13372=CARTESIAN_POINT('Ctrl Pts',(47.5094422967239,201.002028447915,-15.6374322712211));
#13373=CARTESIAN_POINT('Ctrl Pts',(49.9861682551141,200.502028447915,-8.11267584292359));
#13374=CARTESIAN_POINT('Ctrl Pts',(50.0163970020424,200.002028447915,-0.190856796705295));
#13375=CARTESIAN_POINT('Ctrl Pts',(50.0466257489707,199.502028447915,7.730962249513));
#13376=CARTESIAN_POINT('Ctrl Pts',(47.6273982840717,199.002028447915,15.2744010708495));
#13377=CARTESIAN_POINT('Ctrl Pts',(45.2081708191727,198.502028447915,22.817839892186));
#13378=CARTESIAN_POINT('Ctrl Pts',(40.5762979824596,198.002028447915,29.2444941385794));
#13379=CARTESIAN_POINT('Ctrl Pts',(35.9444251457465,197.502028447915,35.6711483849729));
#13380=CARTESIAN_POINT('Ctrl Pts',(29.5533069226325,197.002028447915,40.3519323616533));
#13381=CARTESIAN_POINT('Ctrl Pts',(23.1621886995185,196.502028447915,45.0327163383337));
#13382=CARTESIAN_POINT('Ctrl Pts',(15.6374322712211,196.002028447915,47.5094422967239));
#13383=CARTESIAN_POINT('Ctrl Pts',(8.11267584292359,195.502028447915,49.9861682551141));
#13384=CARTESIAN_POINT('Ctrl Pts',(0.190856796705285,195.002028447915,50.0163970020424));
#13385=CARTESIAN_POINT('Ctrl Pts',(-7.73096224951301,194.502028447915,50.0466257489707));
#13386=CARTESIAN_POINT('Ctrl Pts',(-15.2744010708495,194.002028447915,47.6273982840717));
#13387=CARTESIAN_POINT('Ctrl Pts',(-22.817839892186,193.502028447915,45.2081708191727));
#13388=CARTESIAN_POINT('Ctrl Pts',(-29.2444941385794,193.002028447915,40.5762979824596));
#13389=CARTESIAN_POINT('Ctrl Pts',(-35.6711483849729,192.502028447915,35.9444251457465));
#13390=CARTESIAN_POINT('Ctrl Pts',(-40.3519323616533,192.002028447915,29.5533069226325));
#13391=CARTESIAN_POINT('Ctrl Pts',(-45.0327163383337,191.502028447915,23.1621886995185));
#13392=CARTESIAN_POINT('Ctrl Pts',(-47.5094422967239,191.002028447915,15.6374322712211));
#13393=CARTESIAN_POINT('Ctrl Pts',(-49.9861682551141,190.502028447915,8.11267584292358));
#13394=CARTESIAN_POINT('Ctrl Pts',(-50.0163970020424,190.002028447915,0.190856796705288));
#13395=CARTESIAN_POINT('Ctrl Pts',(-50.0466257489707,189.502028447915,-7.73096224951301));
#13396=CARTESIAN_POINT('Ctrl Pts',(-47.6273982840717,189.002028447915,-15.2744010708495));
#13397=CARTESIAN_POINT('Ctrl Pts',(-45.2081708191727,188.502028447915,-22.817839892186));
#13398=CARTESIAN_POINT('Ctrl Pts',(-40.5762979824596,188.002028447915,-29.2444941385794));
#13399=CARTESIAN_POINT('Ctrl Pts',(-35.9444251457465,187.502028447915,-35.6711483849729));
#13400=CARTESIAN_POINT('Ctrl Pts',(-29.5533069226325,187.002028447915,-40.3519323616533));
#13401=CARTESIAN_POINT('Ctrl Pts',(-23.1621886995185,186.502028447915,-45.0327163383337));
#13402=CARTESIAN_POINT('Ctrl Pts',(-15.6374322712211,186.002028447915,-47.5094422967239));
#13403=CARTESIAN_POINT('Ctrl Pts',(-8.11267584292359,185.502028447915,-49.9861682551141));
#13404=CARTESIAN_POINT('Ctrl Pts',(-0.190856796705292,185.002028447915,
-50.0163970020424));
#13405=CARTESIAN_POINT('Ctrl Pts',(7.730962249513,184.502028447915,-50.0466257489707));
#13406=CARTESIAN_POINT('Ctrl Pts',(15.2744010708495,184.002028447915,-47.6273982840717));
#13407=CARTESIAN_POINT('Ctrl Pts',(22.817839892186,183.502028447915,-45.2081708191727));
#13408=CARTESIAN_POINT('Ctrl Pts',(29.2444941385794,183.002028447915,-40.5762979824596));
#13409=CARTESIAN_POINT('Ctrl Pts',(35.6711483849729,182.502028447915,-35.9444251457465));
#13410=CARTESIAN_POINT('Ctrl Pts',(40.3519323616533,182.002028447915,-29.5533069226325));
#13411=CARTESIAN_POINT('Ctrl Pts',(45.0327163383337,181.502028447915,-23.1621886995185));
#13412=CARTESIAN_POINT('Ctrl Pts',(47.5094422967239,181.002028447915,-15.6374322712211));
#13413=CARTESIAN_POINT('Ctrl Pts',(49.9861682551141,180.502028447915,-8.11267584292359));
#13414=CARTESIAN_POINT('Ctrl Pts',(50.0163970020424,180.002028447915,-0.190856796705295));
#13415=CARTESIAN_POINT('Ctrl Pts',(50.0466257489707,179.502028447915,7.730962249513));
#13416=CARTESIAN_POINT('Ctrl Pts',(47.6273982840717,179.002028447915,15.2744010708495));
#13417=CARTESIAN_POINT('Ctrl Pts',(45.2081708191727,178.502028447915,22.817839892186));
#13418=CARTESIAN_POINT('Ctrl Pts',(40.5762979824596,178.002028447915,29.2444941385794));
#13419=CARTESIAN_POINT('Ctrl Pts',(35.9444251457465,177.502028447915,35.6711483849729));
#13420=CARTESIAN_POINT('Ctrl Pts',(29.5533069226325,177.002028447915,40.3519323616533));
#13421=CARTESIAN_POINT('Ctrl Pts',(23.1621886995185,176.502028447915,45.0327163383337));
#13422=CARTESIAN_POINT('Ctrl Pts',(15.6374322712211,176.002028447915,47.5094422967239));
#13423=CARTESIAN_POINT('Ctrl Pts',(8.11267584292359,175.502028447915,49.9861682551141));
#13424=CARTESIAN_POINT('Ctrl Pts',(0.190856796705285,175.002028447915,50.0163970020424));
#13425=CARTESIAN_POINT('Ctrl Pts',(0.000256710972400845,237.995967593475,
50.0163970020424));
#13426=CARTESIAN_POINT('Ctrl Pts',(-7.92156233524589,237.495967593475,50.0164376610661));
#13427=CARTESIAN_POINT('Ctrl Pts',(-15.4556725243922,236.995967593475,47.5684996184509));
#13428=CARTESIAN_POINT('Ctrl Pts',(-22.9897827135384,236.495967593475,45.1205615758357));
#13429=CARTESIAN_POINT('Ctrl Pts',(-29.3986928470667,235.995967593475,40.4642660629801));
#13430=CARTESIAN_POINT('Ctrl Pts',(-35.8076029805949,235.495967593475,35.8079705501245));
#13431=CARTESIAN_POINT('Ctrl Pts',(-40.4639642811328,234.995967593475,29.3991082141453));
#13432=CARTESIAN_POINT('Ctrl Pts',(-45.1203255816707,234.495967593475,22.990245878166));
#13433=CARTESIAN_POINT('Ctrl Pts',(-47.5683409623447,233.995967593475,15.4561608176784));
#13434=CARTESIAN_POINT('Ctrl Pts',(-50.0163563430187,233.495967593475,7.9220757571907));
#13435=CARTESIAN_POINT('Ctrl Pts',(-50.0163970020424,232.995967593475,0.000256710972403907));
#13436=CARTESIAN_POINT('Ctrl Pts',(-50.0164376610661,232.495967593475,-7.92156233524589));
#13437=CARTESIAN_POINT('Ctrl Pts',(-47.5684996184509,231.995967593475,-15.4556725243922));
#13438=CARTESIAN_POINT('Ctrl Pts',(-45.1205615758357,231.495967593475,-22.9897827135384));
#13439=CARTESIAN_POINT('Ctrl Pts',(-40.4642660629801,230.995967593475,-29.3986928470667));
#13440=CARTESIAN_POINT('Ctrl Pts',(-35.8079705501245,230.495967593475,-35.8076029805949));
#13441=CARTESIAN_POINT('Ctrl Pts',(-29.3991082141453,229.995967593475,-40.4639642811328));
#13442=CARTESIAN_POINT('Ctrl Pts',(-22.9902458781661,229.495967593475,-45.1203255816707));
#13443=CARTESIAN_POINT('Ctrl Pts',(-15.4561608176784,228.995967593475,-47.5683409623447));
#13444=CARTESIAN_POINT('Ctrl Pts',(-7.92207575719071,228.495967593475,-50.0163563430187));
#13445=CARTESIAN_POINT('Ctrl Pts',(-0.00025671097240697,227.995967593475,
-50.0163970020424));
#13446=CARTESIAN_POINT('Ctrl Pts',(7.92156233524589,227.495967593475,-50.0164376610661));
#13447=CARTESIAN_POINT('Ctrl Pts',(15.4556725243922,226.995967593475,-47.5684996184509));
#13448=CARTESIAN_POINT('Ctrl Pts',(22.9897827135384,226.495967593475,-45.1205615758357));
#13449=CARTESIAN_POINT('Ctrl Pts',(29.3986928470667,225.995967593475,-40.4642660629801));
#13450=CARTESIAN_POINT('Ctrl Pts',(35.8076029805949,225.495967593475,-35.8079705501245));
#13451=CARTESIAN_POINT('Ctrl Pts',(40.4639642811328,224.995967593475,-29.3991082141453));
#13452=CARTESIAN_POINT('Ctrl Pts',(45.1203255816707,224.495967593475,-22.9902458781661));
#13453=CARTESIAN_POINT('Ctrl Pts',(47.5683409623447,223.995967593475,-15.4561608176784));
#13454=CARTESIAN_POINT('Ctrl Pts',(50.0163563430187,223.495967593475,-7.92207575719071));
#13455=CARTESIAN_POINT('Ctrl Pts',(50.0163970020424,222.995967593475,-0.000256710972410033));
#13456=CARTESIAN_POINT('Ctrl Pts',(50.0164376610661,222.495967593475,7.92156233524589));
#13457=CARTESIAN_POINT('Ctrl Pts',(47.5684996184509,221.995967593475,15.4556725243922));
#13458=CARTESIAN_POINT('Ctrl Pts',(45.1205615758358,221.495967593475,22.9897827135384));
#13459=CARTESIAN_POINT('Ctrl Pts',(40.4642660629801,220.995967593475,29.3986928470667));
#13460=CARTESIAN_POINT('Ctrl Pts',(35.8079705501245,220.495967593475,35.8076029805949));
#13461=CARTESIAN_POINT('Ctrl Pts',(29.3991082141453,219.995967593475,40.4639642811328));
#13462=CARTESIAN_POINT('Ctrl Pts',(22.9902458781661,219.495967593475,45.1203255816707));
#13463=CARTESIAN_POINT('Ctrl Pts',(15.4561608176784,218.995967593475,47.5683409623447));
#13464=CARTESIAN_POINT('Ctrl Pts',(7.92207575719071,218.495967593475,50.0163563430187));
#13465=CARTESIAN_POINT('Ctrl Pts',(0.000256710972400845,217.995967593475,
50.0163970020424));
#13466=CARTESIAN_POINT('Ctrl Pts',(-7.92156233524589,217.495967593475,50.0164376610661));
#13467=CARTESIAN_POINT('Ctrl Pts',(-15.4556725243922,216.995967593475,47.5684996184509));
#13468=CARTESIAN_POINT('Ctrl Pts',(-22.9897827135384,216.495967593475,45.1205615758357));
#13469=CARTESIAN_POINT('Ctrl Pts',(-29.3986928470667,215.995967593475,40.4642660629801));
#13470=CARTESIAN_POINT('Ctrl Pts',(-35.8076029805949,215.495967593475,35.8079705501245));
#13471=CARTESIAN_POINT('Ctrl Pts',(-40.4639642811328,214.995967593475,29.3991082141453));
#13472=CARTESIAN_POINT('Ctrl Pts',(-45.1203255816707,214.495967593475,22.990245878166));
#13473=CARTESIAN_POINT('Ctrl Pts',(-47.5683409623447,213.995967593475,15.4561608176784));
#13474=CARTESIAN_POINT('Ctrl Pts',(-50.0163563430187,213.495967593475,7.9220757571907));
#13475=CARTESIAN_POINT('Ctrl Pts',(-50.0163970020424,212.995967593475,0.000256710972403907));
#13476=CARTESIAN_POINT('Ctrl Pts',(-50.0164376610661,212.495967593475,-7.92156233524589));
#13477=CARTESIAN_POINT('Ctrl Pts',(-47.5684996184509,211.995967593475,-15.4556725243922));
#13478=CARTESIAN_POINT('Ctrl Pts',(-45.1205615758357,211.495967593475,-22.9897827135384));
#13479=CARTESIAN_POINT('Ctrl Pts',(-40.4642660629801,210.995967593475,-29.3986928470667));
#13480=CARTESIAN_POINT('Ctrl Pts',(-35.8079705501245,210.495967593475,-35.8076029805949));
#13481=CARTESIAN_POINT('Ctrl Pts',(-29.3991082141453,209.995967593475,-40.4639642811328));
#13482=CARTESIAN_POINT('Ctrl Pts',(-22.9902458781661,209.495967593475,-45.1203255816707));
#13483=CARTESIAN_POINT('Ctrl Pts',(-15.4561608176784,208.995967593475,-47.5683409623447));
#13484=CARTESIAN_POINT('Ctrl Pts',(-7.92207575719071,208.495967593475,-50.0163563430187));
#13485=CARTESIAN_POINT('Ctrl Pts',(-0.00025671097240697,207.995967593475,
-50.0163970020424));
#13486=CARTESIAN_POINT('Ctrl Pts',(7.92156233524589,207.495967593475,-50.0164376610661));
#13487=CARTESIAN_POINT('Ctrl Pts',(15.4556725243922,206.995967593475,-47.5684996184509));
#13488=CARTESIAN_POINT('Ctrl Pts',(22.9897827135384,206.495967593475,-45.1205615758357));
#13489=CARTESIAN_POINT('Ctrl Pts',(29.3986928470667,205.995967593475,-40.4642660629801));
#13490=CARTESIAN_POINT('Ctrl Pts',(35.8076029805949,205.495967593475,-35.8079705501245));
#13491=CARTESIAN_POINT('Ctrl Pts',(40.4639642811328,204.995967593475,-29.3991082141453));
#13492=CARTESIAN_POINT('Ctrl Pts',(45.1203255816707,204.495967593475,-22.9902458781661));
#13493=CARTESIAN_POINT('Ctrl Pts',(47.5683409623447,203.995967593475,-15.4561608176784));
#13494=CARTESIAN_POINT('Ctrl Pts',(50.0163563430187,203.495967593475,-7.92207575719071));
#13495=CARTESIAN_POINT('Ctrl Pts',(50.0163970020424,202.995967593475,-0.000256710972410033));
#13496=CARTESIAN_POINT('Ctrl Pts',(50.0164376610661,202.495967593475,7.92156233524589));
#13497=CARTESIAN_POINT('Ctrl Pts',(47.5684996184509,201.995967593475,15.4556725243922));
#13498=CARTESIAN_POINT('Ctrl Pts',(45.1205615758358,201.495967593475,22.9897827135384));
#13499=CARTESIAN_POINT('Ctrl Pts',(40.4642660629801,200.995967593475,29.3986928470667));
#13500=CARTESIAN_POINT('Ctrl Pts',(35.8079705501245,200.495967593475,35.8076029805949));
#13501=CARTESIAN_POINT('Ctrl Pts',(29.3991082141453,199.995967593475,40.4639642811328));
#13502=CARTESIAN_POINT('Ctrl Pts',(22.9902458781661,199.495967593475,45.1203255816707));
#13503=CARTESIAN_POINT('Ctrl Pts',(15.4561608176784,198.995967593475,47.5683409623447));
#13504=CARTESIAN_POINT('Ctrl Pts',(7.92207575719071,198.495967593475,50.0163563430187));
#13505=CARTESIAN_POINT('Ctrl Pts',(0.000256710972400845,197.995967593475,
50.0163970020424));
#13506=CARTESIAN_POINT('Ctrl Pts',(-7.92156233524589,197.495967593475,50.0164376610661));
#13507=CARTESIAN_POINT('Ctrl Pts',(-15.4556725243922,196.995967593475,47.5684996184509));
#13508=CARTESIAN_POINT('Ctrl Pts',(-22.9897827135384,196.495967593475,45.1205615758357));
#13509=CARTESIAN_POINT('Ctrl Pts',(-29.3986928470667,195.995967593475,40.4642660629801));
#13510=CARTESIAN_POINT('Ctrl Pts',(-35.8076029805949,195.495967593475,35.8079705501245));
#13511=CARTESIAN_POINT('Ctrl Pts',(-40.4639642811328,194.995967593475,29.3991082141453));
#13512=CARTESIAN_POINT('Ctrl Pts',(-45.1203255816707,194.495967593475,22.990245878166));
#13513=CARTESIAN_POINT('Ctrl Pts',(-47.5683409623447,193.995967593475,15.4561608176784));
#13514=CARTESIAN_POINT('Ctrl Pts',(-50.0163563430187,193.495967593475,7.9220757571907));
#13515=CARTESIAN_POINT('Ctrl Pts',(-50.0163970020424,192.995967593475,0.000256710972403907));
#13516=CARTESIAN_POINT('Ctrl Pts',(-50.0164376610661,192.495967593475,-7.92156233524589));
#13517=CARTESIAN_POINT('Ctrl Pts',(-47.5684996184509,191.995967593475,-15.4556725243922));
#13518=CARTESIAN_POINT('Ctrl Pts',(-45.1205615758357,191.495967593475,-22.9897827135384));
#13519=CARTESIAN_POINT('Ctrl Pts',(-40.4642660629801,190.995967593475,-29.3986928470667));
#13520=CARTESIAN_POINT('Ctrl Pts',(-35.8079705501245,190.495967593475,-35.8076029805949));
#13521=CARTESIAN_POINT('Ctrl Pts',(-29.3991082141453,189.995967593475,-40.4639642811328));
#13522=CARTESIAN_POINT('Ctrl Pts',(-22.9902458781661,189.495967593475,-45.1203255816707));
#13523=CARTESIAN_POINT('Ctrl Pts',(-15.4561608176784,188.995967593475,-47.5683409623447));
#13524=CARTESIAN_POINT('Ctrl Pts',(-7.92207575719071,188.495967593475,-50.0163563430187));
#13525=CARTESIAN_POINT('Ctrl Pts',(-0.00025671097240697,187.995967593475,
-50.0163970020424));
#13526=CARTESIAN_POINT('Ctrl Pts',(7.92156233524589,187.495967593475,-50.0164376610661));
#13527=CARTESIAN_POINT('Ctrl Pts',(15.4556725243922,186.995967593475,-47.5684996184509));
#13528=CARTESIAN_POINT('Ctrl Pts',(22.9897827135384,186.495967593475,-45.1205615758357));
#13529=CARTESIAN_POINT('Ctrl Pts',(29.3986928470667,185.995967593475,-40.4642660629801));
#13530=CARTESIAN_POINT('Ctrl Pts',(35.8076029805949,185.495967593475,-35.8079705501245));
#13531=CARTESIAN_POINT('Ctrl Pts',(40.4639642811328,184.995967593475,-29.3991082141453));
#13532=CARTESIAN_POINT('Ctrl Pts',(45.1203255816707,184.495967593475,-22.9902458781661));
#13533=CARTESIAN_POINT('Ctrl Pts',(47.5683409623447,183.995967593475,-15.4561608176784));
#13534=CARTESIAN_POINT('Ctrl Pts',(50.0163563430187,183.495967593475,-7.92207575719071));
#13535=CARTESIAN_POINT('Ctrl Pts',(50.0163970020424,182.995967593475,-0.000256710972410033));
#13536=CARTESIAN_POINT('Ctrl Pts',(50.0164376610661,182.495967593475,7.92156233524589));
#13537=CARTESIAN_POINT('Ctrl Pts',(47.5684996184509,181.995967593475,15.4556725243922));
#13538=CARTESIAN_POINT('Ctrl Pts',(45.1205615758358,181.495967593475,22.9897827135384));
#13539=CARTESIAN_POINT('Ctrl Pts',(40.4642660629801,180.995967593475,29.3986928470667));
#13540=CARTESIAN_POINT('Ctrl Pts',(35.8079705501245,180.495967593475,35.8076029805949));
#13541=CARTESIAN_POINT('Ctrl Pts',(29.3991082141453,179.995967593475,40.4639642811328));
#13542=CARTESIAN_POINT('Ctrl Pts',(22.9902458781661,179.495967593475,45.1203255816707));
#13543=CARTESIAN_POINT('Ctrl Pts',(15.4561608176784,178.995967593475,47.5683409623447));
#13544=CARTESIAN_POINT('Ctrl Pts',(7.92207575719071,178.495967593475,50.0163563430187));
#13545=CARTESIAN_POINT('Ctrl Pts',(0.000256710972400845,177.995967593475,
50.0163970020424));
#13546=CARTESIAN_POINT('Origin',(0.,150.,0.));
#13547=CARTESIAN_POINT('',(-5.,100.,-24.4948974278318));
#13548=CARTESIAN_POINT('',(5.,100.,-24.4948974278318));
#13549=CARTESIAN_POINT('Origin',(0.,100.,0.));
#13550=CARTESIAN_POINT('',(5.,150.,-24.4948974278318));
#13551=CARTESIAN_POINT('',(5.,150.,-24.4948974278318));
#13552=CARTESIAN_POINT('',(-5.,150.,-24.4948974278318));
#13553=CARTESIAN_POINT('Origin',(0.,150.,0.));
#13554=CARTESIAN_POINT('',(-5.,150.,-24.4948974278318));
#13555=CARTESIAN_POINT('Origin',(5.,150.,-33.));
#13556=CARTESIAN_POINT('',(5.,100.,-33.));
#13557=CARTESIAN_POINT('',(5.,100.,-24.4948974278318));
#13558=CARTESIAN_POINT('',(5.,150.,-33.));
#13559=CARTESIAN_POINT('',(5.,150.,-33.));
#13560=CARTESIAN_POINT('',(5.,150.,-24.4948974278318));
#13561=CARTESIAN_POINT('Origin',(-5.,150.,-33.));
#13562=CARTESIAN_POINT('',(-5.,100.,-33.));
#13563=CARTESIAN_POINT('',(5.,100.,-33.));
#13564=CARTESIAN_POINT('',(-5.,150.,-33.));
#13565=CARTESIAN_POINT('',(-5.,150.,-33.));
#13566=CARTESIAN_POINT('',(5.,150.,-33.));
#13567=CARTESIAN_POINT('Origin',(-5.,150.,-33.));
#13568=CARTESIAN_POINT('',(-5.,100.,-33.));
#13569=CARTESIAN_POINT('',(-5.,150.,-33.));
#13570=CARTESIAN_POINT('Origin',(0.,150.,0.));
#13571=CARTESIAN_POINT('Origin',(0.,100.,0.));
#13572=CARTESIAN_POINT('',(274.999999999998,612.,-2.51968584885631E-13));
#13573=CARTESIAN_POINT('',(275.704486149526,537.,-19.9875886305758));
#13574=CARTESIAN_POINT('',(275.,872.,6.11682576753421E-14));
#13575=CARTESIAN_POINT('',(276.056510633343,527.006205684712,-19.9751811122038));
#13576=CARTESIAN_POINT('',(275.,537.,-6.72205346941013E-15));
#13577=UNCERTAINTY_MEASURE_WITH_UNIT(LENGTH_MEASURE(0.01),#13595,
'DISTANCE_ACCURACY_VALUE',
'Maximum model space distance between geometric entities at asserted c
onnectivities');
#13578=UNCERTAINTY_MEASURE_WITH_UNIT(LENGTH_MEASURE(0.01),#13595,
'DISTANCE_ACCURACY_VALUE',
'Maximum model space distance between geometric entities at asserted c
onnectivities');
#13579=UNCERTAINTY_MEASURE_WITH_UNIT(LENGTH_MEASURE(0.01),#13595,
'DISTANCE_ACCURACY_VALUE',
'Maximum model space distance between geometric entities at asserted c
onnectivities');
#13580=UNCERTAINTY_MEASURE_WITH_UNIT(LENGTH_MEASURE(0.01),#13595,
'DISTANCE_ACCURACY_VALUE',
'Maximum model space distance between geometric entities at asserted c
onnectivities');
#13581=UNCERTAINTY_MEASURE_WITH_UNIT(LENGTH_MEASURE(0.01),#13595,
'DISTANCE_ACCURACY_VALUE',
'Maximum model space distance between geometric entities at asserted c
onnectivities');
#13582=UNCERTAINTY_MEASURE_WITH_UNIT(LENGTH_MEASURE(0.01),#13595,
'DISTANCE_ACCURACY_VALUE',
'Maximum model space distance between geometric entities at asserted c
onnectivities');
#13583=UNCERTAINTY_MEASURE_WITH_UNIT(LENGTH_MEASURE(0.01),#13595,
'DISTANCE_ACCURACY_VALUE',
'Maximum model space distance between geometric entities at asserted c
onnectivities');
#13584=UNCERTAINTY_MEASURE_WITH_UNIT(LENGTH_MEASURE(0.01),#13595,
'DISTANCE_ACCURACY_VALUE',
'Maximum model space distance between geometric entities at asserted c
onnectivities');
#13585=UNCERTAINTY_MEASURE_WITH_UNIT(LENGTH_MEASURE(0.01),#13595,
'DISTANCE_ACCURACY_VALUE',
'Maximum model space distance between geometric entities at asserted c
onnectivities');
#13586=(
GEOMETRIC_REPRESENTATION_CONTEXT(3)
GLOBAL_UNCERTAINTY_ASSIGNED_CONTEXT((#13577))
GLOBAL_UNIT_ASSIGNED_CONTEXT((#13595,#13597,#13598))
REPRESENTATION_CONTEXT('','3D')
);
#13587=(
GEOMETRIC_REPRESENTATION_CONTEXT(3)
GLOBAL_UNCERTAINTY_ASSIGNED_CONTEXT((#13578))
GLOBAL_UNIT_ASSIGNED_CONTEXT((#13595,#13597,#13598))
REPRESENTATION_CONTEXT('','3D')
);
#13588=(
GEOMETRIC_REPRESENTATION_CONTEXT(3)
GLOBAL_UNCERTAINTY_ASSIGNED_CONTEXT((#13579))
GLOBAL_UNIT_ASSIGNED_CONTEXT((#13595,#13597,#13598))
REPRESENTATION_CONTEXT('','3D')
);
#13589=(
GEOMETRIC_REPRESENTATION_CONTEXT(3)
GLOBAL_UNCERTAINTY_ASSIGNED_CONTEXT((#13580))
GLOBAL_UNIT_ASSIGNED_CONTEXT((#13595,#13597,#13598))
REPRESENTATION_CONTEXT('','3D')
);
#13590=(
GEOMETRIC_REPRESENTATION_CONTEXT(3)
GLOBAL_UNCERTAINTY_ASSIGNED_CONTEXT((#13581))
GLOBAL_UNIT_ASSIGNED_CONTEXT((#13595,#13597,#13598))
REPRESENTATION_CONTEXT('','3D')
);
#13591=(
GEOMETRIC_REPRESENTATION_CONTEXT(3)
GLOBAL_UNCERTAINTY_ASSIGNED_CONTEXT((#13582))
GLOBAL_UNIT_ASSIGNED_CONTEXT((#13595,#13597,#13598))
REPRESENTATION_CONTEXT('','3D')
);
#13592=(
GEOMETRIC_REPRESENTATION_CONTEXT(3)
GLOBAL_UNCERTAINTY_ASSIGNED_CONTEXT((#13583))
GLOBAL_UNIT_ASSIGNED_CONTEXT((#13595,#13597,#13598))
REPRESENTATION_CONTEXT('','3D')
);
#13593=(
GEOMETRIC_REPRESENTATION_CONTEXT(3)
GLOBAL_UNCERTAINTY_ASSIGNED_CONTEXT((#13584))
GLOBAL_UNIT_ASSIGNED_CONTEXT((#13595,#13597,#13598))
REPRESENTATION_CONTEXT('','3D')
);
#13594=(
GEOMETRIC_REPRESENTATION_CONTEXT(3)
GLOBAL_UNCERTAINTY_ASSIGNED_CONTEXT((#13585))
GLOBAL_UNIT_ASSIGNED_CONTEXT((#13595,#13597,#13598))
REPRESENTATION_CONTEXT('','3D')
);
#13595=(
LENGTH_UNIT()
NAMED_UNIT(*)
SI_UNIT(.MILLI.,.METRE.)
);
#13596=(
LENGTH_UNIT()
NAMED_UNIT(*)
SI_UNIT($,.METRE.)
);
#13597=(
NAMED_UNIT(*)
PLANE_ANGLE_UNIT()
SI_UNIT($,.RADIAN.)
);
#13598=(
NAMED_UNIT(*)
SI_UNIT($,.STERADIAN.)
SOLID_ANGLE_UNIT()
);
#13599=SHAPE_DEFINITION_REPRESENTATION(#13607,#13623);
#13600=SHAPE_DEFINITION_REPRESENTATION(#13608,#13624);
#13601=SHAPE_DEFINITION_REPRESENTATION(#13609,#13625);
#13602=SHAPE_DEFINITION_REPRESENTATION(#13610,#13626);
#13603=SHAPE_DEFINITION_REPRESENTATION(#13614,#13627);
#13604=SHAPE_DEFINITION_REPRESENTATION(#13615,#13628);
#13605=SHAPE_DEFINITION_REPRESENTATION(#13616,#13629);
#13606=SHAPE_DEFINITION_REPRESENTATION(#13617,#13630);
#13607=PRODUCT_DEFINITION_SHAPE('',$,#13632);
#13608=PRODUCT_DEFINITION_SHAPE('',$,#13633);
#13609=PRODUCT_DEFINITION_SHAPE('',$,#13634);
#13610=PRODUCT_DEFINITION_SHAPE('',$,#13635);
#13611=PRODUCT_DEFINITION_SHAPE($,$,#37);
#13612=PRODUCT_DEFINITION_SHAPE($,$,#38);
#13613=PRODUCT_DEFINITION_SHAPE($,$,#39);
#13614=PRODUCT_DEFINITION_SHAPE('',$,#13636);
#13615=PRODUCT_DEFINITION_SHAPE('',$,#13637);
#13616=PRODUCT_DEFINITION_SHAPE('',$,#13638);
#13617=PRODUCT_DEFINITION_SHAPE('',$,#13639);
#13618=PRODUCT_DEFINITION_SHAPE($,$,#40);
#13619=PRODUCT_DEFINITION_SHAPE($,$,#41);
#13620=PRODUCT_DEFINITION_SHAPE($,$,#42);
#13621=PRODUCT_DEFINITION_SHAPE($,$,#43);
#13622=PRODUCT_DEFINITION_SHAPE($,$,#44);
#13623=SHAPE_REPRESENTATION('',(#3037,#3271,#3272,#3273,#3274,#3275),#13586);
#13624=SHAPE_REPRESENTATION('',(#3038,#3179,#3180,#3181),#13587);
#13625=SHAPE_REPRESENTATION('',(#3039),#13588);
#13626=SHAPE_REPRESENTATION('',(#3167),#13589);
#13627=SHAPE_REPRESENTATION('',(#3182),#13590);
#13628=SHAPE_REPRESENTATION('',(#3204),#13591);
#13629=SHAPE_REPRESENTATION('',(#3223),#13592);
#13630=SHAPE_REPRESENTATION('',(#3252),#13593);
#13631=PRODUCT_DEFINITION_CONTEXT('part definition',#13657,'design');
#13632=PRODUCT_DEFINITION('MAT-071','MAT-071',#13640,
#13631);
#13633=PRODUCT_DEFINITION('Adjusting Ring Assembly',
'Adjusting Ring Assembly',#13641,#13631);
#13634=PRODUCT_DEFINITION('Ring','Ring',#13642,#13631);
#13635=PRODUCT_DEFINITION('Knurled Grip','Knurled Grip',#13643,#13631);
#13636=PRODUCT_DEFINITION('Discharge Pipe','Discharge Pipe',#13644,#13631);
#13637=PRODUCT_DEFINITION('Hopper','Hopper',#13645,#13631);
#13638=PRODUCT_DEFINITION('Feedback Pipe','Feedback Pipe',#13646,#13631);
#13639=PRODUCT_DEFINITION('Screw Feeder','Screw Feeder',#13647,#13631);
#13640=PRODUCT_DEFINITION_FORMATION('',$,#13659);
#13641=PRODUCT_DEFINITION_FORMATION('',$,#13660);
#13642=PRODUCT_DEFINITION_FORMATION('',$,#13661);
#13643=PRODUCT_DEFINITION_FORMATION('',$,#13662);
#13644=PRODUCT_DEFINITION_FORMATION('',$,#13663);
#13645=PRODUCT_DEFINITION_FORMATION('',$,#13664);
#13646=PRODUCT_DEFINITION_FORMATION('',$,#13665);
#13647=PRODUCT_DEFINITION_FORMATION('',$,#13666);
#13648=PRODUCT_RELATED_PRODUCT_CATEGORY('MAT-071',
'MAT-071',(#13659));
#13649=PRODUCT_RELATED_PRODUCT_CATEGORY('Adjusting Ring Assembly',
'Adjusting Ring Assembly',(#13660));
#13650=PRODUCT_RELATED_PRODUCT_CATEGORY('Ring','Ring',(#13661));
#13651=PRODUCT_RELATED_PRODUCT_CATEGORY('Knurled Grip','Knurled Grip',(#13662));
#13652=PRODUCT_RELATED_PRODUCT_CATEGORY('Discharge Pipe',
'Discharge Pipe',(#13663));
#13653=PRODUCT_RELATED_PRODUCT_CATEGORY('Hopper','Hopper',(#13664));
#13654=PRODUCT_RELATED_PRODUCT_CATEGORY('Feedback Pipe','Feedback Pipe',
(#13665));
#13655=PRODUCT_RELATED_PRODUCT_CATEGORY('Screw Feeder','Screw Feeder',(#13666));
#13656=APPLICATION_PROTOCOL_DEFINITION('international standard',
'automotive_design',2009,#13657);
#13657=APPLICATION_CONTEXT(
'Core Data for Automotive Mechanical Design Process');
#13658=PRODUCT_CONTEXT('part definition',#13657,'mechanical');
#13659=PRODUCT('MAT-071','MAT-071',$,(#13658));
#13660=PRODUCT('Adjusting Ring Assembly','Adjusting Ring Assembly',$,(#13658));
#13661=PRODUCT('Ring','Ring',$,(#13658));
#13662=PRODUCT('Knurled Grip','Knurled Grip',$,(#13658));
#13663=PRODUCT('Discharge Pipe','Discharge Pipe',$,(#13658));
#13664=PRODUCT('Hopper','Hopper',$,(#13658));
#13665=PRODUCT('Feedback Pipe','Feedback Pipe',$,(#13658));
#13666=PRODUCT('Screw Feeder','Screw Feeder',$,(#13658));
#13667=PRESENTATION_STYLE_ASSIGNMENT((#13668));
#13668=SURFACE_STYLE_USAGE(.BOTH.,#13669);
#13669=SURFACE_SIDE_STYLE('',(#13670));
#13670=SURFACE_STYLE_FILL_AREA(#13671);
#13671=FILL_AREA_STYLE('Steel - Satin',(#13672));
#13672=FILL_AREA_STYLE_COLOUR('Steel - Satin',#13673);
#13673=COLOUR_RGB('Steel - Satin',0.627450980392157,0.627450980392157,0.627450980392157);
ENDSEC;
END-ISO-10303-21;
